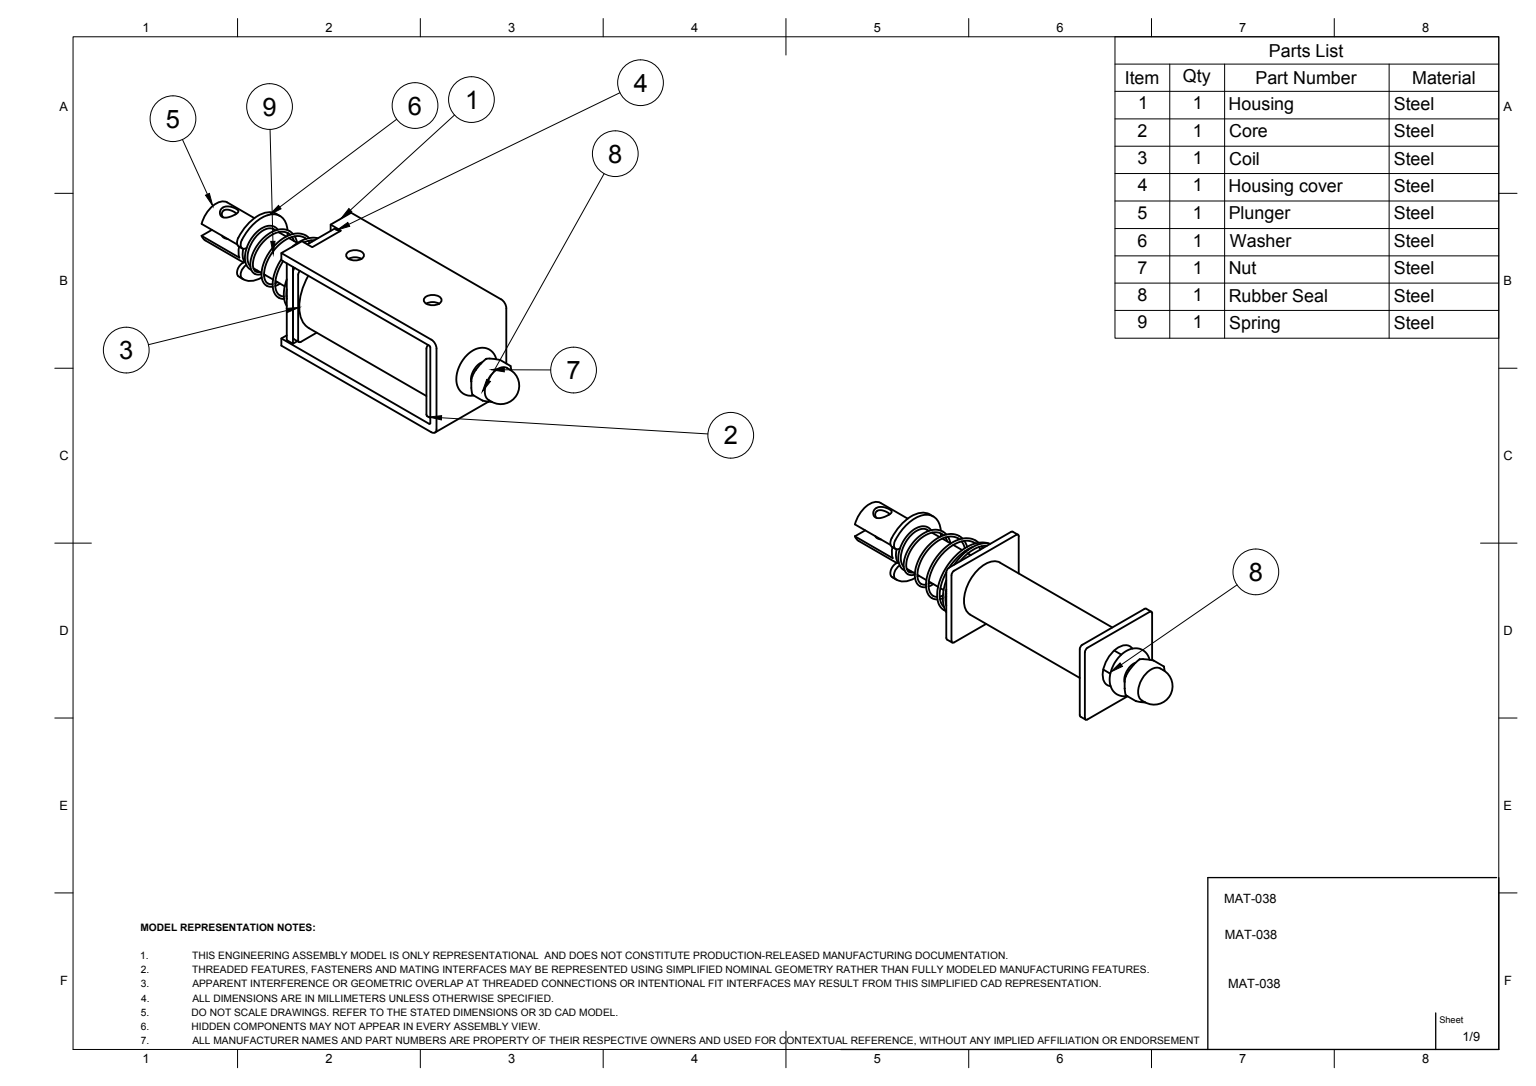
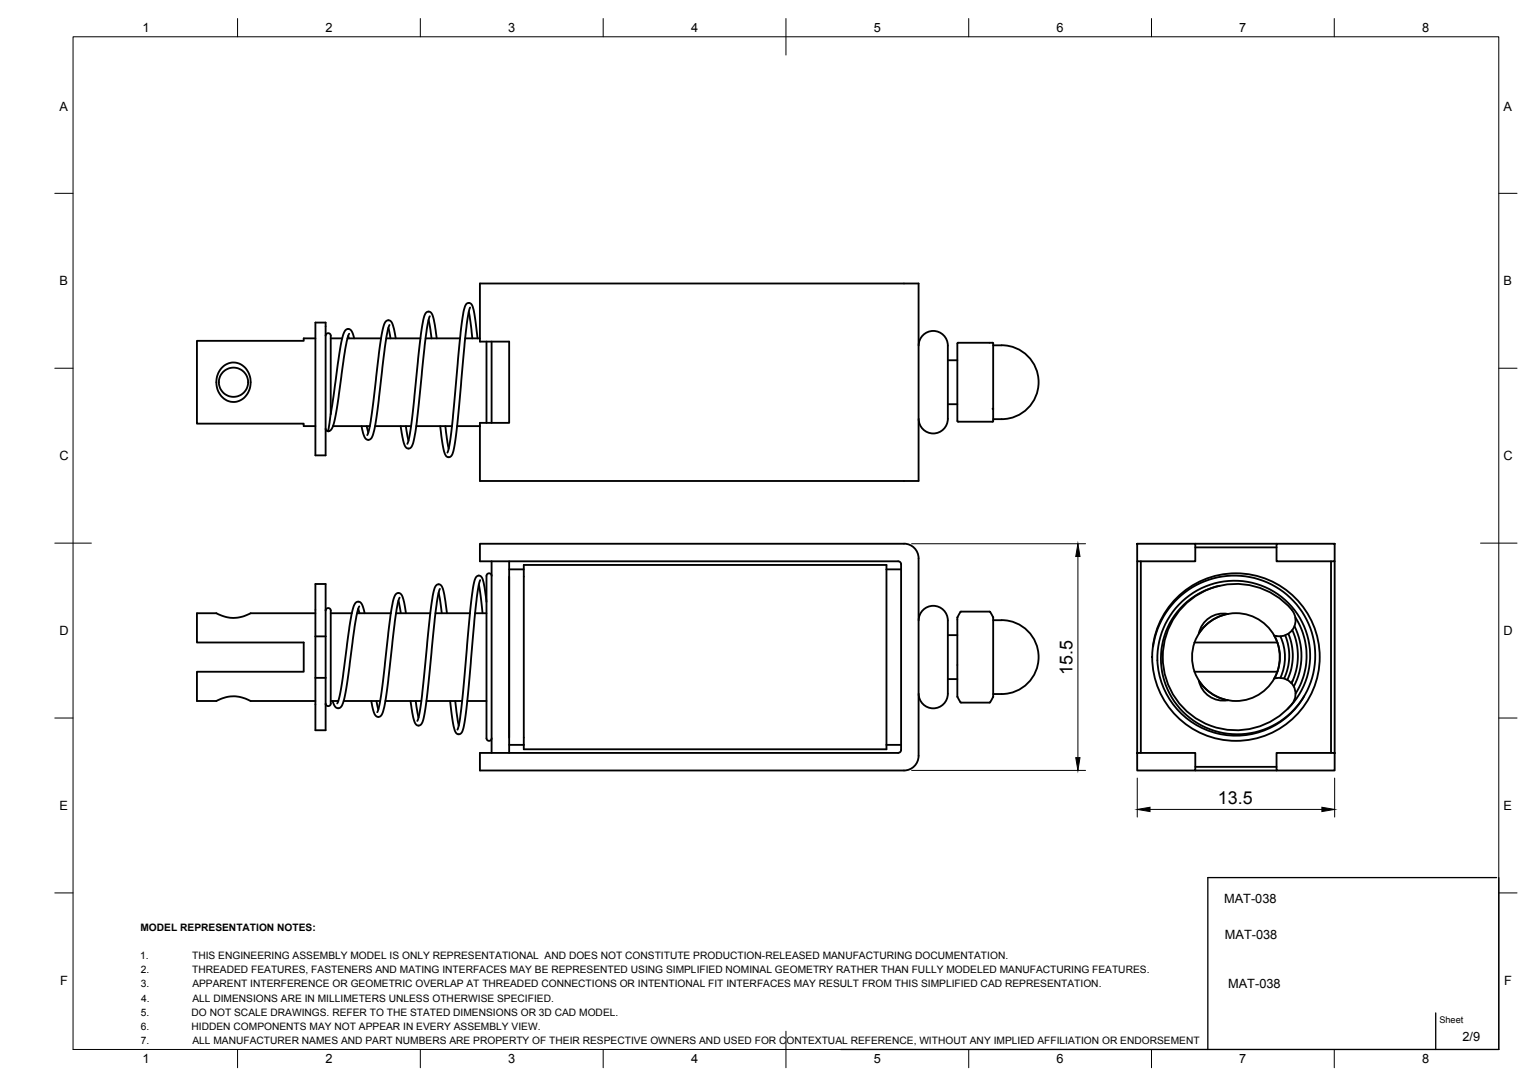
ISO-10303-21;
HEADER;
/* Generated by software containing ST-Developer
 * from STEP Tools, Inc. (www.steptools.com) 
 */

FILE_DESCRIPTION(
/* description */ ('STEP AP214'),
/* implementation_level */ '2;1');

FILE_NAME(
/* name */ 'MAT-038.step',
/* time_stamp */ '2026-11-14T21:32:33-08:00',
/* author */ (''),
/* organization */ (''),
/* preprocessor_version */ 'ST-DEVELOPER v20.2',
/* originating_system */ 'Autodesk Translation Framework v15.17.0.0',
/* authorisation */ '');

FILE_SCHEMA (('AUTOMOTIVE_DESIGN { 1 0 10303 214 3 1 1 }'));
ENDSEC;

DATA;
#10=MECHANICAL_DESIGN_GEOMETRIC_PRESENTATION_REPRESENTATION('',(#177,#178,
#179,#180,#181,#182,#183,#184,#185,#186),#10551);
#11=ITEM_DEFINED_TRANSFORMATION($,$,#3537,#4027);
#12=ITEM_DEFINED_TRANSFORMATION($,$,#3577,#4028);
#13=ITEM_DEFINED_TRANSFORMATION($,$,#3624,#4029);
#14=ITEM_DEFINED_TRANSFORMATION($,$,#3633,#4030);
#15=ITEM_DEFINED_TRANSFORMATION($,$,#3651,#4031);
#16=ITEM_DEFINED_TRANSFORMATION($,$,#3691,#4032);
#17=ITEM_DEFINED_TRANSFORMATION($,$,#3718,#4033);
#18=ITEM_DEFINED_TRANSFORMATION($,$,#4012,#4034);
#19=ITEM_DEFINED_TRANSFORMATION($,$,#4016,#4035);
#20=(
REPRESENTATION_RELATIONSHIP($,$,#10586,#10585)
REPRESENTATION_RELATIONSHIP_WITH_TRANSFORMATION(#11)
SHAPE_REPRESENTATION_RELATIONSHIP()
);
#21=(
REPRESENTATION_RELATIONSHIP($,$,#10587,#10585)
REPRESENTATION_RELATIONSHIP_WITH_TRANSFORMATION(#12)
SHAPE_REPRESENTATION_RELATIONSHIP()
);
#22=(
REPRESENTATION_RELATIONSHIP($,$,#10588,#10585)
REPRESENTATION_RELATIONSHIP_WITH_TRANSFORMATION(#13)
SHAPE_REPRESENTATION_RELATIONSHIP()
);
#23=(
REPRESENTATION_RELATIONSHIP($,$,#10589,#10585)
REPRESENTATION_RELATIONSHIP_WITH_TRANSFORMATION(#14)
SHAPE_REPRESENTATION_RELATIONSHIP()
);
#24=(
REPRESENTATION_RELATIONSHIP($,$,#10590,#10585)
REPRESENTATION_RELATIONSHIP_WITH_TRANSFORMATION(#15)
SHAPE_REPRESENTATION_RELATIONSHIP()
);
#25=(
REPRESENTATION_RELATIONSHIP($,$,#10591,#10585)
REPRESENTATION_RELATIONSHIP_WITH_TRANSFORMATION(#16)
SHAPE_REPRESENTATION_RELATIONSHIP()
);
#26=(
REPRESENTATION_RELATIONSHIP($,$,#10592,#10585)
REPRESENTATION_RELATIONSHIP_WITH_TRANSFORMATION(#17)
SHAPE_REPRESENTATION_RELATIONSHIP()
);
#27=(
REPRESENTATION_RELATIONSHIP($,$,#10593,#10585)
REPRESENTATION_RELATIONSHIP_WITH_TRANSFORMATION(#18)
SHAPE_REPRESENTATION_RELATIONSHIP()
);
#28=(
REPRESENTATION_RELATIONSHIP($,$,#10594,#10585)
REPRESENTATION_RELATIONSHIP_WITH_TRANSFORMATION(#19)
SHAPE_REPRESENTATION_RELATIONSHIP()
);
#29=CONTEXT_DEPENDENT_SHAPE_REPRESENTATION(#20,#10576);
#30=CONTEXT_DEPENDENT_SHAPE_REPRESENTATION(#21,#10577);
#31=CONTEXT_DEPENDENT_SHAPE_REPRESENTATION(#22,#10578);
#32=CONTEXT_DEPENDENT_SHAPE_REPRESENTATION(#23,#10579);
#33=CONTEXT_DEPENDENT_SHAPE_REPRESENTATION(#24,#10580);
#34=CONTEXT_DEPENDENT_SHAPE_REPRESENTATION(#25,#10581);
#35=CONTEXT_DEPENDENT_SHAPE_REPRESENTATION(#26,#10582);
#36=CONTEXT_DEPENDENT_SHAPE_REPRESENTATION(#27,#10583);
#37=CONTEXT_DEPENDENT_SHAPE_REPRESENTATION(#28,#10584);
#38=NEXT_ASSEMBLY_USAGE_OCCURRENCE('Housing:1','Housing:1','Housing:1',
#10596,#10597,'Housing:1');
#39=NEXT_ASSEMBLY_USAGE_OCCURRENCE('Core:1','Core:1','Core:1',#10596,#10598,
'Core:1');
#40=NEXT_ASSEMBLY_USAGE_OCCURRENCE('Coil:1','Coil:1','Coil:1',#10596,#10599,
'Coil:1');
#41=NEXT_ASSEMBLY_USAGE_OCCURRENCE('Housing Cover:1','Housing Cover:1',
'Housing Cover:1',#10596,#10600,'Housing Cover:1');
#42=NEXT_ASSEMBLY_USAGE_OCCURRENCE('Plunger:1','Plunger:1','Plunger:1',
#10596,#10601,'Plunger:1');
#43=NEXT_ASSEMBLY_USAGE_OCCURRENCE('Washer:1','Washer:1','Washer:1',#10596,
#10602,'Washer:1');
#44=NEXT_ASSEMBLY_USAGE_OCCURRENCE('Nut:1','Nut:1','Nut:1',#10596,#10603,
'Nut:1');
#45=NEXT_ASSEMBLY_USAGE_OCCURRENCE('Rubber Seal:1','Rubber Seal:1',
'Rubber Seal:1',#10596,#10604,'Rubber Seal:1');
#46=NEXT_ASSEMBLY_USAGE_OCCURRENCE('Spring:1','Spring:1','Spring:1',#10596,
#10605,'Spring:1');
#47=(
BOUNDED_SURFACE()
B_SPLINE_SURFACE(3,3,((#8436,#8437,#8438,#8439,#8440,#8441,#8442,#8443,
#8444,#8445,#8446,#8447,#8448,#8449,#8450,#8451,#8452,#8453,#8454,#8455,
#8456,#8457,#8458,#8459,#8460,#8461,#8462,#8463,#8464,#8465,#8466,#8467,
#8468,#8469,#8470,#8471,#8472,#8473,#8474,#8475,#8476,#8477,#8478,#8479,
#8480,#8481,#8482,#8483,#8484,#8485,#8486,#8487,#8488,#8489,#8490,#8491,
#8492,#8493,#8494,#8495,#8496,#8497,#8498,#8499,#8500,#8501,#8502,#8503,
#8504,#8505,#8506,#8507,#8508,#8509,#8510,#8511,#8512,#8513,#8514,#8515,
#8516,#8517,#8518,#8519,#8520,#8521,#8522,#8523,#8524,#8525,#8526,#8527,
#8528,#8529,#8530,#8531,#8532,#8533,#8534,#8535,#8536,#8537,#8538,#8539,
#8540,#8541,#8542,#8543,#8544,#8545,#8546,#8547,#8548,#8549,#8550,#8551,
#8552,#8553,#8554,#8555,#8556,#8557,#8558,#8559,#8560,#8561,#8562,#8563,
#8564,#8565),(#8566,#8567,#8568,#8569,#8570,#8571,#8572,#8573,#8574,#8575,
#8576,#8577,#8578,#8579,#8580,#8581,#8582,#8583,#8584,#8585,#8586,#8587,
#8588,#8589,#8590,#8591,#8592,#8593,#8594,#8595,#8596,#8597,#8598,#8599,
#8600,#8601,#8602,#8603,#8604,#8605,#8606,#8607,#8608,#8609,#8610,#8611,
#8612,#8613,#8614,#8615,#8616,#8617,#8618,#8619,#8620,#8621,#8622,#8623,
#8624,#8625,#8626,#8627,#8628,#8629,#8630,#8631,#8632,#8633,#8634,#8635,
#8636,#8637,#8638,#8639,#8640,#8641,#8642,#8643,#8644,#8645,#8646,#8647,
#8648,#8649,#8650,#8651,#8652,#8653,#8654,#8655,#8656,#8657,#8658,#8659,
#8660,#8661,#8662,#8663,#8664,#8665,#8666,#8667,#8668,#8669,#8670,#8671,
#8672,#8673,#8674,#8675,#8676,#8677,#8678,#8679,#8680,#8681,#8682,#8683,
#8684,#8685,#8686,#8687,#8688,#8689,#8690,#8691,#8692,#8693,#8694,#8695),
(#8696,#8697,#8698,#8699,#8700,#8701,#8702,#8703,#8704,#8705,#8706,#8707,
#8708,#8709,#8710,#8711,#8712,#8713,#8714,#8715,#8716,#8717,#8718,#8719,
#8720,#8721,#8722,#8723,#8724,#8725,#8726,#8727,#8728,#8729,#8730,#8731,
#8732,#8733,#8734,#8735,#8736,#8737,#8738,#8739,#8740,#8741,#8742,#8743,
#8744,#8745,#8746,#8747,#8748,#8749,#8750,#8751,#8752,#8753,#8754,#8755,
#8756,#8757,#8758,#8759,#8760,#8761,#8762,#8763,#8764,#8765,#8766,#8767,
#8768,#8769,#8770,#8771,#8772,#8773,#8774,#8775,#8776,#8777,#8778,#8779,
#8780,#8781,#8782,#8783,#8784,#8785,#8786,#8787,#8788,#8789,#8790,#8791,
#8792,#8793,#8794,#8795,#8796,#8797,#8798,#8799,#8800,#8801,#8802,#8803,
#8804,#8805,#8806,#8807,#8808,#8809,#8810,#8811,#8812,#8813,#8814,#8815,
#8816,#8817,#8818,#8819,#8820,#8821,#8822,#8823,#8824,#8825),(#8826,#8827,
#8828,#8829,#8830,#8831,#8832,#8833,#8834,#8835,#8836,#8837,#8838,#8839,
#8840,#8841,#8842,#8843,#8844,#8845,#8846,#8847,#8848,#8849,#8850,#8851,
#8852,#8853,#8854,#8855,#8856,#8857,#8858,#8859,#8860,#8861,#8862,#8863,
#8864,#8865,#8866,#8867,#8868,#8869,#8870,#8871,#8872,#8873,#8874,#8875,
#8876,#8877,#8878,#8879,#8880,#8881,#8882,#8883,#8884,#8885,#8886,#8887,
#8888,#8889,#8890,#8891,#8892,#8893,#8894,#8895,#8896,#8897,#8898,#8899,
#8900,#8901,#8902,#8903,#8904,#8905,#8906,#8907,#8908,#8909,#8910,#8911,
#8912,#8913,#8914,#8915,#8916,#8917,#8918,#8919,#8920,#8921,#8922,#8923,
#8924,#8925,#8926,#8927,#8928,#8929,#8930,#8931,#8932,#8933,#8934,#8935,
#8936,#8937,#8938,#8939,#8940,#8941,#8942,#8943,#8944,#8945,#8946,#8947,
#8948,#8949,#8950,#8951,#8952,#8953,#8954,#8955),(#8956,#8957,#8958,#8959,
#8960,#8961,#8962,#8963,#8964,#8965,#8966,#8967,#8968,#8969,#8970,#8971,
#8972,#8973,#8974,#8975,#8976,#8977,#8978,#8979,#8980,#8981,#8982,#8983,
#8984,#8985,#8986,#8987,#8988,#8989,#8990,#8991,#8992,#8993,#8994,#8995,
#8996,#8997,#8998,#8999,#9000,#9001,#9002,#9003,#9004,#9005,#9006,#9007,
#9008,#9009,#9010,#9011,#9012,#9013,#9014,#9015,#9016,#9017,#9018,#9019,
#9020,#9021,#9022,#9023,#9024,#9025,#9026,#9027,#9028,#9029,#9030,#9031,
#9032,#9033,#9034,#9035,#9036,#9037,#9038,#9039,#9040,#9041,#9042,#9043,
#9044,#9045,#9046,#9047,#9048,#9049,#9050,#9051,#9052,#9053,#9054,#9055,
#9056,#9057,#9058,#9059,#9060,#9061,#9062,#9063,#9064,#9065,#9066,#9067,
#9068,#9069,#9070,#9071,#9072,#9073,#9074,#9075,#9076,#9077,#9078,#9079,
#9080,#9081,#9082,#9083,#9084,#9085),(#9086,#9087,#9088,#9089,#9090,#9091,
#9092,#9093,#9094,#9095,#9096,#9097,#9098,#9099,#9100,#9101,#9102,#9103,
#9104,#9105,#9106,#9107,#9108,#9109,#9110,#9111,#9112,#9113,#9114,#9115,
#9116,#9117,#9118,#9119,#9120,#9121,#9122,#9123,#9124,#9125,#9126,#9127,
#9128,#9129,#9130,#9131,#9132,#9133,#9134,#9135,#9136,#9137,#9138,#9139,
#9140,#9141,#9142,#9143,#9144,#9145,#9146,#9147,#9148,#9149,#9150,#9151,
#9152,#9153,#9154,#9155,#9156,#9157,#9158,#9159,#9160,#9161,#9162,#9163,
#9164,#9165,#9166,#9167,#9168,#9169,#9170,#9171,#9172,#9173,#9174,#9175,
#9176,#9177,#9178,#9179,#9180,#9181,#9182,#9183,#9184,#9185,#9186,#9187,
#9188,#9189,#9190,#9191,#9192,#9193,#9194,#9195,#9196,#9197,#9198,#9199,
#9200,#9201,#9202,#9203,#9204,#9205,#9206,#9207,#9208,#9209,#9210,#9211,
#9212,#9213,#9214,#9215),(#9216,#9217,#9218,#9219,#9220,#9221,#9222,#9223,
#9224,#9225,#9226,#9227,#9228,#9229,#9230,#9231,#9232,#9233,#9234,#9235,
#9236,#9237,#9238,#9239,#9240,#9241,#9242,#9243,#9244,#9245,#9246,#9247,
#9248,#9249,#9250,#9251,#9252,#9253,#9254,#9255,#9256,#9257,#9258,#9259,
#9260,#9261,#9262,#9263,#9264,#9265,#9266,#9267,#9268,#9269,#9270,#9271,
#9272,#9273,#9274,#9275,#9276,#9277,#9278,#9279,#9280,#9281,#9282,#9283,
#9284,#9285,#9286,#9287,#9288,#9289,#9290,#9291,#9292,#9293,#9294,#9295,
#9296,#9297,#9298,#9299,#9300,#9301,#9302,#9303,#9304,#9305,#9306,#9307,
#9308,#9309,#9310,#9311,#9312,#9313,#9314,#9315,#9316,#9317,#9318,#9319,
#9320,#9321,#9322,#9323,#9324,#9325,#9326,#9327,#9328,#9329,#9330,#9331,
#9332,#9333,#9334,#9335,#9336,#9337,#9338,#9339,#9340,#9341,#9342,#9343,
#9344,#9345)),.UNSPECIFIED.,.T.,.F.,.F.)
B_SPLINE_SURFACE_WITH_KNOTS((4,3,4),(4,2,2,2,2,2,2,2,2,2,2,2,2,2,2,2,2,
2,2,2,2,2,2,2,2,2,2,2,2,2,2,2,2,2,2,2,2,2,2,2,2,2,2,2,2,2,2,2,2,2,2,2,2,
2,2,2,2,2,2,2,2,2,2,2,4),(0.,0.5,1.),(-1.6716721247158E-5,0.015625,0.03125,
0.046875,0.0625,0.078125,0.09375,0.109375,0.125,0.140625,0.15625,0.171875,
0.1875,0.203125,0.21875,0.234375,0.25,0.265625,0.28125,0.296875,0.3125,
0.328125,0.34375,0.359375,0.375,0.390625,0.40625,0.421875,0.4375,0.453125,
0.46875,0.484375,0.5,0.515625,0.53125,0.546875,0.5625,0.578125,0.59375,
0.609375,0.625,0.640625,0.65625,0.671875,0.6875,0.703125,0.71875,0.734375,
0.75,0.765625,0.78125,0.796875,0.8125,0.828125,0.84375,0.859375,0.875,0.890625,
0.90625,0.921875,0.9375,0.953125,0.96875,0.984375,1.),.UNSPECIFIED.)
GEOMETRIC_REPRESENTATION_ITEM()
RATIONAL_B_SPLINE_SURFACE(((1.,1.,1.,1.,1.,1.,1.,1.,1.,1.,1.,1.,1.,1.,1.,
1.,1.,1.,1.,1.,1.,1.,1.,1.,1.,1.,1.,1.,1.,1.,1.,1.,1.,1.,1.,1.,1.,1.,1.,
1.,1.,1.,1.,1.,1.,1.,1.,1.,1.,1.,1.,1.,1.,1.,1.,1.,1.,1.,1.,1.,1.,1.,1.,
1.,1.,1.,1.,1.,1.,1.,1.,1.,1.,1.,1.,1.,1.,1.,1.,1.,1.,1.,1.,1.,1.,1.,1.,
1.,1.,1.,1.,1.,1.,1.,1.,1.,1.,1.,1.,1.,1.,1.,1.,1.,1.,1.,1.,1.,1.,1.,1.,
1.,1.,1.,1.,1.,1.,1.,1.,1.,1.,1.,1.,1.,1.,1.,1.,1.,1.,1.),(0.333333333333334,
0.333333333333333,0.333333333333333,0.333333333333333,0.333333333333333,
0.333333333333333,0.333333333333333,0.333333333333333,0.333333333333333,
0.333333333333333,0.333333333333333,0.333333333333333,0.333333333333333,
0.333333333333333,0.333333333333333,0.333333333333333,0.333333333333333,
0.333333333333333,0.333333333333333,0.333333333333333,0.333333333333333,
0.333333333333333,0.333333333333333,0.333333333333333,0.333333333333333,
0.333333333333333,0.333333333333333,0.333333333333333,0.333333333333333,
0.333333333333333,0.333333333333333,0.333333333333333,0.333333333333333,
0.333333333333333,0.333333333333333,0.333333333333333,0.333333333333333,
0.333333333333333,0.333333333333333,0.333333333333333,0.333333333333333,
0.333333333333333,0.333333333333333,0.333333333333333,0.333333333333333,
0.333333333333333,0.333333333333333,0.333333333333333,0.333333333333333,
0.333333333333333,0.333333333333333,0.333333333333333,0.333333333333333,
0.333333333333333,0.333333333333333,0.333333333333333,0.333333333333333,
0.333333333333333,0.333333333333333,0.333333333333333,0.333333333333333,
0.333333333333333,0.333333333333333,0.333333333333333,0.333333333333333,
0.333333333333333,0.333333333333333,0.333333333333333,0.333333333333333,
0.333333333333333,0.333333333333333,0.333333333333333,0.333333333333333,
0.333333333333333,0.333333333333333,0.333333333333333,0.333333333333333,
0.333333333333333,0.333333333333333,0.333333333333333,0.333333333333333,
0.333333333333333,0.333333333333333,0.333333333333333,0.333333333333333,
0.333333333333333,0.333333333333333,0.333333333333333,0.333333333333333,
0.333333333333333,0.333333333333333,0.333333333333333,0.333333333333333,
0.333333333333333,0.333333333333333,0.333333333333333,0.333333333333333,
0.333333333333333,0.333333333333333,0.333333333333333,0.333333333333333,
0.333333333333333,0.333333333333333,0.333333333333333,0.333333333333333,
0.333333333333333,0.333333333333333,0.333333333333333,0.333333333333333,
0.333333333333333,0.333333333333333,0.333333333333333,0.333333333333333,
0.333333333333333,0.333333333333333,0.333333333333333,0.333333333333333,
0.333333333333333,0.333333333333333,0.333333333333333,0.333333333333333,
0.333333333333333,0.333333333333333,0.333333333333333,0.333333333333333,
0.333333333333333,0.333333333333333,0.333333333333333,0.333333333333333,
0.333333333333333),(0.333333333333334,0.333333333333333,0.333333333333333,
0.333333333333333,0.333333333333333,0.333333333333333,0.333333333333333,
0.333333333333333,0.333333333333333,0.333333333333333,0.333333333333333,
0.333333333333333,0.333333333333333,0.333333333333333,0.333333333333333,
0.333333333333333,0.333333333333333,0.333333333333333,0.333333333333333,
0.333333333333333,0.333333333333333,0.333333333333333,0.333333333333333,
0.333333333333333,0.333333333333333,0.333333333333333,0.333333333333333,
0.333333333333333,0.333333333333333,0.333333333333333,0.333333333333333,
0.333333333333333,0.333333333333333,0.333333333333333,0.333333333333333,
0.333333333333333,0.333333333333333,0.333333333333333,0.333333333333333,
0.333333333333333,0.333333333333333,0.333333333333333,0.333333333333333,
0.333333333333333,0.333333333333333,0.333333333333333,0.333333333333333,
0.333333333333333,0.333333333333333,0.333333333333333,0.333333333333333,
0.333333333333333,0.333333333333333,0.333333333333333,0.333333333333333,
0.333333333333333,0.333333333333333,0.333333333333333,0.333333333333333,
0.333333333333333,0.333333333333333,0.333333333333333,0.333333333333333,
0.333333333333333,0.333333333333333,0.333333333333333,0.333333333333333,
0.333333333333333,0.333333333333333,0.333333333333333,0.333333333333333,
0.333333333333333,0.333333333333333,0.333333333333333,0.333333333333333,
0.333333333333333,0.333333333333333,0.333333333333333,0.333333333333333,
0.333333333333333,0.333333333333333,0.333333333333333,0.333333333333333,
0.333333333333333,0.333333333333333,0.333333333333333,0.333333333333333,
0.333333333333333,0.333333333333333,0.333333333333333,0.333333333333333,
0.333333333333333,0.333333333333333,0.333333333333333,0.333333333333333,
0.333333333333333,0.333333333333333,0.333333333333333,0.333333333333333,
0.333333333333333,0.333333333333333,0.333333333333333,0.333333333333333,
0.333333333333333,0.333333333333333,0.333333333333333,0.333333333333333,
0.333333333333333,0.333333333333333,0.333333333333333,0.333333333333333,
0.333333333333333,0.333333333333333,0.333333333333333,0.333333333333333,
0.333333333333333,0.333333333333333,0.333333333333333,0.333333333333333,
0.333333333333333,0.333333333333333,0.333333333333333,0.333333333333333,
0.333333333333333,0.333333333333333,0.333333333333333,0.333333333333333,
0.333333333333333,0.333333333333333,0.333333333333333),(1.,1.,1.,1.,1.,
1.,1.,1.,1.,1.,1.,1.,1.,1.,1.,1.,1.,1.,1.,1.,1.,1.,1.,1.,1.,1.,1.,1.,1.,
1.,1.,1.,1.,1.,1.,1.,1.,1.,1.,1.,1.,1.,1.,1.,1.,1.,1.,1.,1.,1.,1.,1.,1.,
1.,1.,1.,1.,1.,1.,1.,1.,1.,1.,1.,1.,1.,1.,1.,1.,1.,1.,1.,1.,1.,1.,1.,1.,
1.,1.,1.,1.,1.,1.,1.,1.,1.,1.,1.,1.,1.,1.,1.,1.,1.,1.,1.,1.,1.,1.,1.,1.,
1.,1.,1.,1.,1.,1.,1.,1.,1.,1.,1.,1.,1.,1.,1.,1.,1.,1.,1.,1.,1.,1.,1.,1.,
1.,1.,1.,1.,1.),(0.333333333333334,0.333333333333333,0.333333333333333,
0.333333333333333,0.333333333333333,0.333333333333333,0.333333333333333,
0.333333333333333,0.333333333333333,0.333333333333333,0.333333333333333,
0.333333333333333,0.333333333333333,0.333333333333333,0.333333333333333,
0.333333333333333,0.333333333333333,0.333333333333333,0.333333333333333,
0.333333333333333,0.333333333333333,0.333333333333333,0.333333333333333,
0.333333333333333,0.333333333333333,0.333333333333333,0.333333333333333,
0.333333333333333,0.333333333333333,0.333333333333333,0.333333333333333,
0.333333333333333,0.333333333333333,0.333333333333333,0.333333333333333,
0.333333333333333,0.333333333333333,0.333333333333333,0.333333333333333,
0.333333333333333,0.333333333333333,0.333333333333333,0.333333333333333,
0.333333333333333,0.333333333333333,0.333333333333333,0.333333333333333,
0.333333333333333,0.333333333333333,0.333333333333333,0.333333333333333,
0.333333333333333,0.333333333333333,0.333333333333333,0.333333333333333,
0.333333333333333,0.333333333333333,0.333333333333333,0.333333333333333,
0.333333333333333,0.333333333333333,0.333333333333333,0.333333333333333,
0.333333333333333,0.333333333333333,0.333333333333333,0.333333333333333,
0.333333333333333,0.333333333333333,0.333333333333333,0.333333333333333,
0.333333333333333,0.333333333333333,0.333333333333333,0.333333333333333,
0.333333333333333,0.333333333333333,0.333333333333333,0.333333333333333,
0.333333333333333,0.333333333333333,0.333333333333333,0.333333333333333,
0.333333333333333,0.333333333333333,0.333333333333333,0.333333333333333,
0.333333333333333,0.333333333333333,0.333333333333333,0.333333333333333,
0.333333333333333,0.333333333333333,0.333333333333333,0.333333333333333,
0.333333333333333,0.333333333333333,0.333333333333333,0.333333333333333,
0.333333333333333,0.333333333333333,0.333333333333333,0.333333333333333,
0.333333333333333,0.333333333333333,0.333333333333333,0.333333333333333,
0.333333333333333,0.333333333333333,0.333333333333333,0.333333333333333,
0.333333333333333,0.333333333333333,0.333333333333333,0.333333333333333,
0.333333333333333,0.333333333333333,0.333333333333333,0.333333333333333,
0.333333333333333,0.333333333333333,0.333333333333333,0.333333333333333,
0.333333333333333,0.333333333333333,0.333333333333333,0.333333333333333,
0.333333333333333,0.333333333333333,0.333333333333333),(0.333333333333334,
0.333333333333333,0.333333333333333,0.333333333333333,0.333333333333333,
0.333333333333333,0.333333333333333,0.333333333333333,0.333333333333333,
0.333333333333333,0.333333333333333,0.333333333333333,0.333333333333333,
0.333333333333333,0.333333333333333,0.333333333333333,0.333333333333333,
0.333333333333333,0.333333333333333,0.333333333333333,0.333333333333333,
0.333333333333333,0.333333333333333,0.333333333333333,0.333333333333333,
0.333333333333333,0.333333333333333,0.333333333333333,0.333333333333333,
0.333333333333333,0.333333333333333,0.333333333333333,0.333333333333333,
0.333333333333333,0.333333333333333,0.333333333333333,0.333333333333333,
0.333333333333333,0.333333333333333,0.333333333333333,0.333333333333333,
0.333333333333333,0.333333333333333,0.333333333333333,0.333333333333333,
0.333333333333333,0.333333333333333,0.333333333333333,0.333333333333333,
0.333333333333333,0.333333333333333,0.333333333333333,0.333333333333333,
0.333333333333333,0.333333333333333,0.333333333333333,0.333333333333333,
0.333333333333333,0.333333333333333,0.333333333333333,0.333333333333333,
0.333333333333333,0.333333333333333,0.333333333333333,0.333333333333333,
0.333333333333333,0.333333333333333,0.333333333333333,0.333333333333333,
0.333333333333333,0.333333333333333,0.333333333333333,0.333333333333333,
0.333333333333333,0.333333333333333,0.333333333333333,0.333333333333333,
0.333333333333333,0.333333333333333,0.333333333333333,0.333333333333333,
0.333333333333333,0.333333333333333,0.333333333333333,0.333333333333333,
0.333333333333333,0.333333333333333,0.333333333333333,0.333333333333333,
0.333333333333333,0.333333333333333,0.333333333333333,0.333333333333333,
0.333333333333333,0.333333333333333,0.333333333333333,0.333333333333333,
0.333333333333333,0.333333333333333,0.333333333333333,0.333333333333333,
0.333333333333333,0.333333333333333,0.333333333333333,0.333333333333333,
0.333333333333333,0.333333333333333,0.333333333333333,0.333333333333333,
0.333333333333333,0.333333333333333,0.333333333333333,0.333333333333333,
0.333333333333333,0.333333333333333,0.333333333333333,0.333333333333333,
0.333333333333333,0.333333333333333,0.333333333333333,0.333333333333333,
0.333333333333333,0.333333333333333,0.333333333333333,0.333333333333333,
0.333333333333333,0.333333333333333,0.333333333333333,0.333333333333333,
0.333333333333333),(1.,1.,1.,1.,1.,1.,1.,1.,1.,1.,1.,1.,1.,1.,1.,1.,1.,
1.,1.,1.,1.,1.,1.,1.,1.,1.,1.,1.,1.,1.,1.,1.,1.,1.,1.,1.,1.,1.,1.,1.,1.,
1.,1.,1.,1.,1.,1.,1.,1.,1.,1.,1.,1.,1.,1.,1.,1.,1.,1.,1.,1.,1.,1.,1.,1.,
1.,1.,1.,1.,1.,1.,1.,1.,1.,1.,1.,1.,1.,1.,1.,1.,1.,1.,1.,1.,1.,1.,1.,1.,
1.,1.,1.,1.,1.,1.,1.,1.,1.,1.,1.,1.,1.,1.,1.,1.,1.,1.,1.,1.,1.,1.,1.,1.,
1.,1.,1.,1.,1.,1.,1.,1.,1.,1.,1.,1.,1.,1.,1.,1.,1.)))
REPRESENTATION_ITEM('')
SURFACE()
);
#48=(
BOUNDED_SURFACE()
B_SPLINE_SURFACE(3,3,((#9609,#9610,#9611,#9612,#9613,#9614,#9615,#9616,
#9617,#9618,#9619,#9620,#9621,#9622,#9623,#9624,#9625,#9626,#9627,#9628,
#9629,#9630,#9631,#9632,#9633,#9634,#9635,#9636,#9637,#9638,#9639,#9640,
#9641,#9642,#9643,#9644,#9645,#9646,#9647,#9648,#9649,#9650,#9651,#9652,
#9653,#9654,#9655,#9656,#9657,#9658,#9659,#9660,#9661,#9662,#9663,#9664,
#9665,#9666,#9667,#9668,#9669,#9670,#9671,#9672,#9673,#9674,#9675,#9676,
#9677,#9678,#9679,#9680,#9681,#9682,#9683,#9684,#9685,#9686,#9687,#9688,
#9689,#9690,#9691,#9692,#9693,#9694,#9695,#9696,#9697,#9698,#9699,#9700,
#9701,#9702,#9703,#9704,#9705,#9706,#9707,#9708,#9709,#9710,#9711,#9712,
#9713,#9714,#9715,#9716,#9717,#9718,#9719,#9720,#9721,#9722,#9723,#9724,
#9725,#9726,#9727,#9728,#9729,#9730,#9731,#9732,#9733,#9734,#9735,#9736,
#9737,#9738),(#9739,#9740,#9741,#9742,#9743,#9744,#9745,#9746,#9747,#9748,
#9749,#9750,#9751,#9752,#9753,#9754,#9755,#9756,#9757,#9758,#9759,#9760,
#9761,#9762,#9763,#9764,#9765,#9766,#9767,#9768,#9769,#9770,#9771,#9772,
#9773,#9774,#9775,#9776,#9777,#9778,#9779,#9780,#9781,#9782,#9783,#9784,
#9785,#9786,#9787,#9788,#9789,#9790,#9791,#9792,#9793,#9794,#9795,#9796,
#9797,#9798,#9799,#9800,#9801,#9802,#9803,#9804,#9805,#9806,#9807,#9808,
#9809,#9810,#9811,#9812,#9813,#9814,#9815,#9816,#9817,#9818,#9819,#9820,
#9821,#9822,#9823,#9824,#9825,#9826,#9827,#9828,#9829,#9830,#9831,#9832,
#9833,#9834,#9835,#9836,#9837,#9838,#9839,#9840,#9841,#9842,#9843,#9844,
#9845,#9846,#9847,#9848,#9849,#9850,#9851,#9852,#9853,#9854,#9855,#9856,
#9857,#9858,#9859,#9860,#9861,#9862,#9863,#9864,#9865,#9866,#9867,#9868),
(#9869,#9870,#9871,#9872,#9873,#9874,#9875,#9876,#9877,#9878,#9879,#9880,
#9881,#9882,#9883,#9884,#9885,#9886,#9887,#9888,#9889,#9890,#9891,#9892,
#9893,#9894,#9895,#9896,#9897,#9898,#9899,#9900,#9901,#9902,#9903,#9904,
#9905,#9906,#9907,#9908,#9909,#9910,#9911,#9912,#9913,#9914,#9915,#9916,
#9917,#9918,#9919,#9920,#9921,#9922,#9923,#9924,#9925,#9926,#9927,#9928,
#9929,#9930,#9931,#9932,#9933,#9934,#9935,#9936,#9937,#9938,#9939,#9940,
#9941,#9942,#9943,#9944,#9945,#9946,#9947,#9948,#9949,#9950,#9951,#9952,
#9953,#9954,#9955,#9956,#9957,#9958,#9959,#9960,#9961,#9962,#9963,#9964,
#9965,#9966,#9967,#9968,#9969,#9970,#9971,#9972,#9973,#9974,#9975,#9976,
#9977,#9978,#9979,#9980,#9981,#9982,#9983,#9984,#9985,#9986,#9987,#9988,
#9989,#9990,#9991,#9992,#9993,#9994,#9995,#9996,#9997,#9998),(#9999,#10000,
#10001,#10002,#10003,#10004,#10005,#10006,#10007,#10008,#10009,#10010,#10011,
#10012,#10013,#10014,#10015,#10016,#10017,#10018,#10019,#10020,#10021,#10022,
#10023,#10024,#10025,#10026,#10027,#10028,#10029,#10030,#10031,#10032,#10033,
#10034,#10035,#10036,#10037,#10038,#10039,#10040,#10041,#10042,#10043,#10044,
#10045,#10046,#10047,#10048,#10049,#10050,#10051,#10052,#10053,#10054,#10055,
#10056,#10057,#10058,#10059,#10060,#10061,#10062,#10063,#10064,#10065,#10066,
#10067,#10068,#10069,#10070,#10071,#10072,#10073,#10074,#10075,#10076,#10077,
#10078,#10079,#10080,#10081,#10082,#10083,#10084,#10085,#10086,#10087,#10088,
#10089,#10090,#10091,#10092,#10093,#10094,#10095,#10096,#10097,#10098,#10099,
#10100,#10101,#10102,#10103,#10104,#10105,#10106,#10107,#10108,#10109,#10110,
#10111,#10112,#10113,#10114,#10115,#10116,#10117,#10118,#10119,#10120,#10121,
#10122,#10123,#10124,#10125,#10126,#10127,#10128),(#10129,#10130,#10131,
#10132,#10133,#10134,#10135,#10136,#10137,#10138,#10139,#10140,#10141,#10142,
#10143,#10144,#10145,#10146,#10147,#10148,#10149,#10150,#10151,#10152,#10153,
#10154,#10155,#10156,#10157,#10158,#10159,#10160,#10161,#10162,#10163,#10164,
#10165,#10166,#10167,#10168,#10169,#10170,#10171,#10172,#10173,#10174,#10175,
#10176,#10177,#10178,#10179,#10180,#10181,#10182,#10183,#10184,#10185,#10186,
#10187,#10188,#10189,#10190,#10191,#10192,#10193,#10194,#10195,#10196,#10197,
#10198,#10199,#10200,#10201,#10202,#10203,#10204,#10205,#10206,#10207,#10208,
#10209,#10210,#10211,#10212,#10213,#10214,#10215,#10216,#10217,#10218,#10219,
#10220,#10221,#10222,#10223,#10224,#10225,#10226,#10227,#10228,#10229,#10230,
#10231,#10232,#10233,#10234,#10235,#10236,#10237,#10238,#10239,#10240,#10241,
#10242,#10243,#10244,#10245,#10246,#10247,#10248,#10249,#10250,#10251,#10252,
#10253,#10254,#10255,#10256,#10257,#10258),(#10259,#10260,#10261,#10262,
#10263,#10264,#10265,#10266,#10267,#10268,#10269,#10270,#10271,#10272,#10273,
#10274,#10275,#10276,#10277,#10278,#10279,#10280,#10281,#10282,#10283,#10284,
#10285,#10286,#10287,#10288,#10289,#10290,#10291,#10292,#10293,#10294,#10295,
#10296,#10297,#10298,#10299,#10300,#10301,#10302,#10303,#10304,#10305,#10306,
#10307,#10308,#10309,#10310,#10311,#10312,#10313,#10314,#10315,#10316,#10317,
#10318,#10319,#10320,#10321,#10322,#10323,#10324,#10325,#10326,#10327,#10328,
#10329,#10330,#10331,#10332,#10333,#10334,#10335,#10336,#10337,#10338,#10339,
#10340,#10341,#10342,#10343,#10344,#10345,#10346,#10347,#10348,#10349,#10350,
#10351,#10352,#10353,#10354,#10355,#10356,#10357,#10358,#10359,#10360,#10361,
#10362,#10363,#10364,#10365,#10366,#10367,#10368,#10369,#10370,#10371,#10372,
#10373,#10374,#10375,#10376,#10377,#10378,#10379,#10380,#10381,#10382,#10383,
#10384,#10385,#10386,#10387,#10388),(#10389,#10390,#10391,#10392,#10393,
#10394,#10395,#10396,#10397,#10398,#10399,#10400,#10401,#10402,#10403,#10404,
#10405,#10406,#10407,#10408,#10409,#10410,#10411,#10412,#10413,#10414,#10415,
#10416,#10417,#10418,#10419,#10420,#10421,#10422,#10423,#10424,#10425,#10426,
#10427,#10428,#10429,#10430,#10431,#10432,#10433,#10434,#10435,#10436,#10437,
#10438,#10439,#10440,#10441,#10442,#10443,#10444,#10445,#10446,#10447,#10448,
#10449,#10450,#10451,#10452,#10453,#10454,#10455,#10456,#10457,#10458,#10459,
#10460,#10461,#10462,#10463,#10464,#10465,#10466,#10467,#10468,#10469,#10470,
#10471,#10472,#10473,#10474,#10475,#10476,#10477,#10478,#10479,#10480,#10481,
#10482,#10483,#10484,#10485,#10486,#10487,#10488,#10489,#10490,#10491,#10492,
#10493,#10494,#10495,#10496,#10497,#10498,#10499,#10500,#10501,#10502,#10503,
#10504,#10505,#10506,#10507,#10508,#10509,#10510,#10511,#10512,#10513,#10514,
#10515,#10516,#10517,#10518)),.UNSPECIFIED.,.T.,.F.,.F.)
B_SPLINE_SURFACE_WITH_KNOTS((4,3,4),(4,2,2,2,2,2,2,2,2,2,2,2,2,2,2,2,2,
2,2,2,2,2,2,2,2,2,2,2,2,2,2,2,2,2,2,2,2,2,2,2,2,2,2,2,2,2,2,2,2,2,2,2,2,
2,2,2,2,2,2,2,2,2,2,2,4),(0.,0.5,1.),(0.,0.015625,0.03125,0.046875,0.0625,
0.078125,0.09375,0.109375,0.125,0.140625,0.15625,0.171875,0.1875,0.203125,
0.21875,0.234375,0.25,0.265625,0.28125,0.296875,0.3125,0.328125,0.34375,
0.359375,0.375,0.390625,0.40625,0.421875,0.4375,0.453125,0.46875,0.484375,
0.5,0.515625,0.53125,0.546875,0.5625,0.578125,0.59375,0.609375,0.625,0.640625,
0.65625,0.671875,0.6875,0.703125,0.71875,0.734375,0.75,0.765625,0.78125,
0.796875,0.8125,0.828125,0.84375,0.859375,0.875,0.890625,0.90625,0.921875,
0.9375,0.953125,0.96875,0.984375,1.),.UNSPECIFIED.)
GEOMETRIC_REPRESENTATION_ITEM()
RATIONAL_B_SPLINE_SURFACE(((1.,1.,1.,1.,1.,1.,1.,1.,1.,1.,1.,1.,1.,1.,1.,
1.,1.,1.,1.,1.,1.,1.,1.,1.,1.,1.,1.,1.,1.,1.,1.,1.,1.,1.,1.,1.,1.,1.,1.,
1.,1.,1.,1.,1.,1.,1.,1.,1.,1.,1.,1.,1.,1.,1.,1.,1.,1.,1.,1.,1.,1.,1.,1.,
1.,1.,1.,1.,1.,1.,1.,1.,1.,1.,1.,1.,1.,1.,1.,1.,1.,1.,1.,1.,1.,1.,1.,1.,
1.,1.,1.,1.,1.,1.,1.,1.,1.,1.,1.,1.,1.,1.,1.,1.,1.,1.,1.,1.,1.,1.,1.,1.,
1.,1.,1.,1.,1.,1.,1.,1.,1.,1.,1.,1.,1.,1.,1.,1.,1.,1.,1.),(0.333333333333333,
0.333333333333333,0.333333333333333,0.333333333333333,0.333333333333333,
0.333333333333333,0.333333333333333,0.333333333333333,0.333333333333333,
0.333333333333333,0.333333333333333,0.333333333333333,0.333333333333333,
0.333333333333333,0.333333333333333,0.333333333333333,0.333333333333333,
0.333333333333333,0.333333333333333,0.333333333333333,0.333333333333333,
0.333333333333333,0.333333333333333,0.333333333333333,0.333333333333333,
0.333333333333333,0.333333333333333,0.333333333333333,0.333333333333333,
0.333333333333333,0.333333333333333,0.333333333333333,0.333333333333333,
0.333333333333333,0.333333333333333,0.333333333333333,0.333333333333333,
0.333333333333333,0.333333333333333,0.333333333333333,0.333333333333333,
0.333333333333333,0.333333333333333,0.333333333333333,0.333333333333333,
0.333333333333333,0.333333333333333,0.333333333333333,0.333333333333333,
0.333333333333333,0.333333333333333,0.333333333333333,0.333333333333333,
0.333333333333333,0.333333333333333,0.333333333333333,0.333333333333333,
0.333333333333333,0.333333333333333,0.333333333333333,0.333333333333333,
0.333333333333333,0.333333333333333,0.333333333333333,0.333333333333333,
0.333333333333333,0.333333333333333,0.333333333333333,0.333333333333333,
0.333333333333333,0.333333333333333,0.333333333333333,0.333333333333333,
0.333333333333333,0.333333333333333,0.333333333333333,0.333333333333333,
0.333333333333333,0.333333333333333,0.333333333333333,0.333333333333333,
0.333333333333333,0.333333333333333,0.333333333333333,0.333333333333333,
0.333333333333333,0.333333333333333,0.333333333333333,0.333333333333333,
0.333333333333333,0.333333333333333,0.333333333333333,0.333333333333333,
0.333333333333333,0.333333333333333,0.333333333333333,0.333333333333333,
0.333333333333333,0.333333333333333,0.333333333333333,0.333333333333333,
0.333333333333333,0.333333333333333,0.333333333333333,0.333333333333333,
0.333333333333333,0.333333333333333,0.333333333333333,0.333333333333333,
0.333333333333333,0.333333333333333,0.333333333333333,0.333333333333333,
0.333333333333333,0.333333333333333,0.333333333333333,0.333333333333333,
0.333333333333333,0.333333333333333,0.333333333333333,0.333333333333333,
0.333333333333333,0.333333333333333,0.333333333333333,0.333333333333333,
0.333333333333333,0.333333333333333,0.333333333333333,0.333333333333333,
0.333333333333333),(0.333333333333333,0.333333333333333,0.333333333333333,
0.333333333333333,0.333333333333333,0.333333333333333,0.333333333333333,
0.333333333333333,0.333333333333333,0.333333333333333,0.333333333333333,
0.333333333333333,0.333333333333333,0.333333333333333,0.333333333333333,
0.333333333333333,0.333333333333333,0.333333333333333,0.333333333333333,
0.333333333333333,0.333333333333333,0.333333333333333,0.333333333333333,
0.333333333333333,0.333333333333333,0.333333333333333,0.333333333333333,
0.333333333333333,0.333333333333333,0.333333333333333,0.333333333333333,
0.333333333333333,0.333333333333333,0.333333333333333,0.333333333333333,
0.333333333333333,0.333333333333333,0.333333333333333,0.333333333333333,
0.333333333333333,0.333333333333333,0.333333333333333,0.333333333333333,
0.333333333333333,0.333333333333333,0.333333333333333,0.333333333333333,
0.333333333333333,0.333333333333333,0.333333333333333,0.333333333333333,
0.333333333333333,0.333333333333333,0.333333333333333,0.333333333333333,
0.333333333333333,0.333333333333333,0.333333333333333,0.333333333333333,
0.333333333333333,0.333333333333333,0.333333333333333,0.333333333333333,
0.333333333333333,0.333333333333333,0.333333333333333,0.333333333333333,
0.333333333333333,0.333333333333333,0.333333333333333,0.333333333333333,
0.333333333333333,0.333333333333333,0.333333333333333,0.333333333333333,
0.333333333333333,0.333333333333333,0.333333333333333,0.333333333333333,
0.333333333333333,0.333333333333333,0.333333333333333,0.333333333333333,
0.333333333333333,0.333333333333333,0.333333333333333,0.333333333333333,
0.333333333333333,0.333333333333333,0.333333333333333,0.333333333333333,
0.333333333333333,0.333333333333333,0.333333333333333,0.333333333333333,
0.333333333333333,0.333333333333333,0.333333333333333,0.333333333333333,
0.333333333333333,0.333333333333333,0.333333333333333,0.333333333333333,
0.333333333333333,0.333333333333333,0.333333333333333,0.333333333333333,
0.333333333333333,0.333333333333333,0.333333333333333,0.333333333333333,
0.333333333333333,0.333333333333333,0.333333333333333,0.333333333333333,
0.333333333333333,0.333333333333333,0.333333333333333,0.333333333333333,
0.333333333333333,0.333333333333333,0.333333333333333,0.333333333333333,
0.333333333333333,0.333333333333333,0.333333333333333,0.333333333333333,
0.333333333333333,0.333333333333333,0.333333333333333),(1.,1.,1.,1.,1.,
1.,1.,1.,1.,1.,1.,1.,1.,1.,1.,1.,1.,1.,1.,1.,1.,1.,1.,1.,1.,1.,1.,1.,1.,
1.,1.,1.,1.,1.,1.,1.,1.,1.,1.,1.,1.,1.,1.,1.,1.,1.,1.,1.,1.,1.,1.,1.,1.,
1.,1.,1.,1.,1.,1.,1.,1.,1.,1.,1.,1.,1.,1.,1.,1.,1.,1.,1.,1.,1.,1.,1.,1.,
1.,1.,1.,1.,1.,1.,1.,1.,1.,1.,1.,1.,1.,1.,1.,1.,1.,1.,1.,1.,1.,1.,1.,1.,
1.,1.,1.,1.,1.,1.,1.,1.,1.,1.,1.,1.,1.,1.,1.,1.,1.,1.,1.,1.,1.,1.,1.,1.,
1.,1.,1.,1.,1.),(0.333333333333333,0.333333333333333,0.333333333333333,
0.333333333333333,0.333333333333333,0.333333333333333,0.333333333333333,
0.333333333333333,0.333333333333333,0.333333333333333,0.333333333333333,
0.333333333333333,0.333333333333333,0.333333333333333,0.333333333333333,
0.333333333333333,0.333333333333333,0.333333333333333,0.333333333333333,
0.333333333333333,0.333333333333333,0.333333333333333,0.333333333333333,
0.333333333333333,0.333333333333333,0.333333333333333,0.333333333333333,
0.333333333333333,0.333333333333333,0.333333333333333,0.333333333333333,
0.333333333333333,0.333333333333333,0.333333333333333,0.333333333333333,
0.333333333333333,0.333333333333333,0.333333333333333,0.333333333333333,
0.333333333333333,0.333333333333333,0.333333333333333,0.333333333333333,
0.333333333333333,0.333333333333333,0.333333333333333,0.333333333333333,
0.333333333333333,0.333333333333333,0.333333333333333,0.333333333333333,
0.333333333333333,0.333333333333333,0.333333333333333,0.333333333333333,
0.333333333333333,0.333333333333333,0.333333333333333,0.333333333333333,
0.333333333333333,0.333333333333333,0.333333333333333,0.333333333333333,
0.333333333333333,0.333333333333333,0.333333333333333,0.333333333333333,
0.333333333333333,0.333333333333333,0.333333333333333,0.333333333333333,
0.333333333333333,0.333333333333333,0.333333333333333,0.333333333333333,
0.333333333333333,0.333333333333333,0.333333333333333,0.333333333333333,
0.333333333333333,0.333333333333333,0.333333333333333,0.333333333333333,
0.333333333333333,0.333333333333333,0.333333333333333,0.333333333333333,
0.333333333333333,0.333333333333333,0.333333333333333,0.333333333333333,
0.333333333333333,0.333333333333333,0.333333333333333,0.333333333333333,
0.333333333333333,0.333333333333333,0.333333333333333,0.333333333333333,
0.333333333333333,0.333333333333333,0.333333333333333,0.333333333333333,
0.333333333333333,0.333333333333333,0.333333333333333,0.333333333333333,
0.333333333333333,0.333333333333333,0.333333333333333,0.333333333333333,
0.333333333333333,0.333333333333333,0.333333333333333,0.333333333333333,
0.333333333333333,0.333333333333333,0.333333333333333,0.333333333333333,
0.333333333333333,0.333333333333333,0.333333333333333,0.333333333333333,
0.333333333333333,0.333333333333333,0.333333333333333,0.333333333333333,
0.333333333333333,0.333333333333333,0.333333333333333),(0.333333333333333,
0.333333333333333,0.333333333333333,0.333333333333333,0.333333333333333,
0.333333333333333,0.333333333333333,0.333333333333333,0.333333333333333,
0.333333333333333,0.333333333333333,0.333333333333333,0.333333333333333,
0.333333333333333,0.333333333333333,0.333333333333333,0.333333333333333,
0.333333333333333,0.333333333333333,0.333333333333333,0.333333333333333,
0.333333333333333,0.333333333333333,0.333333333333333,0.333333333333333,
0.333333333333333,0.333333333333333,0.333333333333333,0.333333333333333,
0.333333333333333,0.333333333333333,0.333333333333333,0.333333333333333,
0.333333333333333,0.333333333333333,0.333333333333333,0.333333333333333,
0.333333333333333,0.333333333333333,0.333333333333333,0.333333333333333,
0.333333333333333,0.333333333333333,0.333333333333333,0.333333333333333,
0.333333333333333,0.333333333333333,0.333333333333333,0.333333333333333,
0.333333333333333,0.333333333333333,0.333333333333333,0.333333333333333,
0.333333333333333,0.333333333333333,0.333333333333333,0.333333333333333,
0.333333333333333,0.333333333333333,0.333333333333333,0.333333333333333,
0.333333333333333,0.333333333333333,0.333333333333333,0.333333333333333,
0.333333333333333,0.333333333333333,0.333333333333333,0.333333333333333,
0.333333333333333,0.333333333333333,0.333333333333333,0.333333333333333,
0.333333333333333,0.333333333333333,0.333333333333333,0.333333333333333,
0.333333333333333,0.333333333333333,0.333333333333333,0.333333333333333,
0.333333333333333,0.333333333333333,0.333333333333333,0.333333333333333,
0.333333333333333,0.333333333333333,0.333333333333333,0.333333333333333,
0.333333333333333,0.333333333333333,0.333333333333333,0.333333333333333,
0.333333333333333,0.333333333333333,0.333333333333333,0.333333333333333,
0.333333333333333,0.333333333333333,0.333333333333333,0.333333333333333,
0.333333333333333,0.333333333333333,0.333333333333333,0.333333333333333,
0.333333333333333,0.333333333333333,0.333333333333333,0.333333333333333,
0.333333333333333,0.333333333333333,0.333333333333333,0.333333333333333,
0.333333333333333,0.333333333333333,0.333333333333333,0.333333333333333,
0.333333333333333,0.333333333333333,0.333333333333333,0.333333333333333,
0.333333333333333,0.333333333333333,0.333333333333333,0.333333333333333,
0.333333333333333,0.333333333333333,0.333333333333333,0.333333333333333,
0.333333333333333),(1.,1.,1.,1.,1.,1.,1.,1.,1.,1.,1.,1.,1.,1.,1.,1.,1.,
1.,1.,1.,1.,1.,1.,1.,1.,1.,1.,1.,1.,1.,1.,1.,1.,1.,1.,1.,1.,1.,1.,1.,1.,
1.,1.,1.,1.,1.,1.,1.,1.,1.,1.,1.,1.,1.,1.,1.,1.,1.,1.,1.,1.,1.,1.,1.,1.,
1.,1.,1.,1.,1.,1.,1.,1.,1.,1.,1.,1.,1.,1.,1.,1.,1.,1.,1.,1.,1.,1.,1.,1.,
1.,1.,1.,1.,1.,1.,1.,1.,1.,1.,1.,1.,1.,1.,1.,1.,1.,1.,1.,1.,1.,1.,1.,1.,
1.,1.,1.,1.,1.,1.,1.,1.,1.,1.,1.,1.,1.,1.,1.,1.,1.)))
REPRESENTATION_ITEM('')
SURFACE()
);
#49=ELLIPSE('',#4023,0.175430953951623,0.175001932698577);
#50=SPHERICAL_SURFACE('',#3737,2.525);
#51=SPHERICAL_SURFACE('',#3742,6.);
#52=SPHERICAL_SURFACE('',#3746,6.);
#53=SPHERICAL_SURFACE('',#3750,6.);
#54=SPHERICAL_SURFACE('',#3754,6.);
#55=SPHERICAL_SURFACE('',#3800,6.);
#56=SPHERICAL_SURFACE('',#3803,6.);
#57=SPHERICAL_SURFACE('',#3807,6.);
#58=SPHERICAL_SURFACE('',#3811,6.);
#59=SPHERICAL_SURFACE('',#3814,6.);
#60=SPHERICAL_SURFACE('',#3817,6.);
#61=SPHERICAL_SURFACE('',#3821,6.);
#62=SPHERICAL_SURFACE('',#3825,6.);
#63=SPHERICAL_SURFACE('',#3829,0.05);
#64=SPHERICAL_SURFACE('',#3845,0.05);
#65=SPHERICAL_SURFACE('',#3847,0.05);
#66=SPHERICAL_SURFACE('',#3849,0.05);
#67=SPHERICAL_SURFACE('',#3851,0.05);
#68=SPHERICAL_SURFACE('',#3873,0.05);
#69=SPHERICAL_SURFACE('',#3875,0.05);
#70=SPHERICAL_SURFACE('',#3877,0.05);
#71=SPHERICAL_SURFACE('',#3879,0.05);
#72=SPHERICAL_SURFACE('',#3881,0.05);
#73=SPHERICAL_SURFACE('',#3883,0.05);
#74=SPHERICAL_SURFACE('',#3903,0.05);
#75=SPHERICAL_SURFACE('',#3905,0.05);
#76=SPHERICAL_SURFACE('',#3907,0.05);
#77=SPHERICAL_SURFACE('',#3909,0.05);
#78=SPHERICAL_SURFACE('',#3911,0.05);
#79=SPHERICAL_SURFACE('',#3913,0.05);
#80=SPHERICAL_SURFACE('',#3936,0.05);
#81=SPHERICAL_SURFACE('',#3938,0.05);
#82=SPHERICAL_SURFACE('',#3941,0.05);
#83=SPHERICAL_SURFACE('',#3943,0.05);
#84=SPHERICAL_SURFACE('',#3945,0.05);
#85=SPHERICAL_SURFACE('',#3946,0.05);
#86=SPHERICAL_SURFACE('',#3948,0.05);
#87=SPHERICAL_SURFACE('',#3968,0.05);
#88=SPHERICAL_SURFACE('',#3970,0.05);
#89=SPHERICAL_SURFACE('',#3972,0.05);
#90=SPHERICAL_SURFACE('',#3974,0.05);
#91=SPHERICAL_SURFACE('',#3990,0.05);
#92=SPHERICAL_SURFACE('',#3992,0.05);
#93=SPHERICAL_SURFACE('',#3994,0.05);
#94=SPHERICAL_SURFACE('',#3996,0.05);
#95=SPHERICAL_SURFACE('',#4006,0.05);
#96=SPHERICAL_SURFACE('',#4008,0.05);
#97=TOROIDAL_SURFACE('',#3724,2.70416345659799,0.05);
#98=TOROIDAL_SURFACE('',#3732,2.70416345659799,0.05);
#99=TOROIDAL_SURFACE('',#3835,2.70416345659799,0.05);
#100=TOROIDAL_SURFACE('',#3837,5.32728824074688,0.05);
#101=TOROIDAL_SURFACE('',#3840,5.32728824074688,0.05);
#102=TOROIDAL_SURFACE('',#3842,5.32728824074688,0.05);
#103=TOROIDAL_SURFACE('',#3854,5.32728824074688,0.05);
#104=TOROIDAL_SURFACE('',#3856,2.70416345659799,0.05);
#105=TOROIDAL_SURFACE('',#3862,5.32728824074688,0.05);
#106=TOROIDAL_SURFACE('',#3868,5.32728824074688,0.05);
#107=TOROIDAL_SURFACE('',#3887,5.32728824074688,0.05);
#108=TOROIDAL_SURFACE('',#3890,5.32728824074688,0.05);
#109=TOROIDAL_SURFACE('',#3892,5.32728824074688,0.05);
#110=TOROIDAL_SURFACE('',#3894,2.70416345659799,0.05);
#111=TOROIDAL_SURFACE('',#3896,2.70416345659799,0.05);
#112=TOROIDAL_SURFACE('',#3898,5.32728824074688,0.05);
#113=TOROIDAL_SURFACE('',#3900,5.32728824074688,0.05);
#114=TOROIDAL_SURFACE('',#3915,5.32728824074688,0.05);
#115=TOROIDAL_SURFACE('',#3917,2.70416345659799,0.05);
#116=TOROIDAL_SURFACE('',#3919,2.70416345659799,0.05);
#117=TOROIDAL_SURFACE('',#3926,5.32728824074688,0.05);
#118=TOROIDAL_SURFACE('',#3933,5.32728824074688,0.05);
#119=TOROIDAL_SURFACE('',#3954,5.32728824074688,0.05);
#120=TOROIDAL_SURFACE('',#3956,5.32728824074688,0.05);
#121=TOROIDAL_SURFACE('',#3958,5.32728824074688,0.05);
#122=TOROIDAL_SURFACE('',#3960,2.70416345659799,0.05);
#123=TOROIDAL_SURFACE('',#3962,5.32728824074688,0.05);
#124=TOROIDAL_SURFACE('',#3964,5.32728824074688,0.05);
#125=TOROIDAL_SURFACE('',#3966,5.32728824074688,0.05);
#126=TOROIDAL_SURFACE('',#3978,5.32728824074688,0.05);
#127=TOROIDAL_SURFACE('',#3985,5.32728824074688,0.05);
#128=TOROIDAL_SURFACE('',#3998,5.32728824074688,0.05);
#129=TOROIDAL_SURFACE('',#4000,2.70416345659799,0.05);
#130=TOROIDAL_SURFACE('',#4002,2.70416345659799,0.05);
#131=TOROIDAL_SURFACE('',#4004,5.32728824074688,0.05);
#132=TOROIDAL_SURFACE('',#4013,2.5,1.);
#133=TOROIDAL_SURFACE('',#4017,5.55,0.175);
#134=TOROIDAL_SURFACE('',#4020,3.17573472959676,0.175);
#135=CONICAL_SURFACE('',#3666,1.14999999999999,0.785398163397463);
#136=CONICAL_SURFACE('',#3674,1.99999999999999,0.0977269073587189);
#137=CONICAL_SURFACE('',#3719,1.15,0.785398163397453);
#138=B_SPLINE_CURVE_WITH_KNOTS('',3,(#6086,#6087,#6088,#6089,#6090,#6091,
#6092,#6093,#6094,#6095,#6096,#6097,#6098,#6099,#6100,#6101,#6102,#6103,
#6104,#6105,#6106,#6107),.UNSPECIFIED.,.F.,.F.,(4,2,2,2,2,2,2,2,2,2,4),
(-0.398476386723121,-0.363413449903791,-0.328945780906488,-0.279734113540581,
-0.238759142767186,-0.202537073889496,-0.166278974820396,-0.125546922866738,
-0.0748109574930432,-0.0377065280884949,0.),.UNSPECIFIED.);
#139=B_SPLINE_CURVE_WITH_KNOTS('',3,(#6111,#6112,#6113,#6114),
 .UNSPECIFIED.,.F.,.F.,(4,4),(-0.320868204557424,-0.320859930375376),
 .UNSPECIFIED.);
#140=B_SPLINE_CURVE_WITH_KNOTS('',3,(#6116,#6117,#6118,#6119,#6120,#6121,
#6122,#6123,#6124,#6125,#6126,#6127,#6128,#6129,#6130,#6131,#6132,#6133,
#6134,#6135,#6136,#6137,#6138,#6139),.UNSPECIFIED.,.F.,.F.,(4,2,2,2,2,2,
2,2,2,2,2,4),(-0.320859930375376,-0.303821997926792,-0.286725131861031,
-0.252375001979002,-0.231369369238555,-0.194211321091721,-0.160393271457449,
-0.126524952102273,-0.0894197007003378,-0.0475320396288663,-0.0237192939459634,
-1.00000035202497E-6),.UNSPECIFIED.);
#141=B_SPLINE_CURVE_WITH_KNOTS('',3,(#6635,#6636,#6637,#6638,#6639,#6640,
#6641,#6642,#6643,#6644,#6645,#6646,#6647,#6648,#6649,#6650,#6651,#6652,
#6653,#6654,#6655,#6656),.UNSPECIFIED.,.F.,.F.,(4,2,2,2,2,2,2,2,2,2,4),
(-0.398476386717938,-0.363413449898109,-0.328945780900276,-0.279734113534564,
-0.238759142762232,-0.202537073885482,-0.166278974817291,-0.125546922864936,
-0.074810957492591,-0.0377065280884339,0.),.UNSPECIFIED.);
#142=B_SPLINE_CURVE_WITH_KNOTS('',3,(#6660,#6661,#6662,#6663),
 .UNSPECIFIED.,.F.,.F.,(4,4),(-0.320868204532271,-0.320859930350223),
 .UNSPECIFIED.);
#143=B_SPLINE_CURVE_WITH_KNOTS('',3,(#6665,#6666,#6667,#6668,#6669,#6670,
#6671,#6672,#6673,#6674,#6675,#6676,#6677,#6678,#6679,#6680,#6681,#6682,
#6683,#6684,#6685,#6686,#6687,#6688),.UNSPECIFIED.,.F.,.F.,(4,2,2,2,2,2,
2,2,2,2,2,4),(-0.320859930350223,-0.303821997902903,-0.286725131838533,
-0.252375001959359,-0.23136936922067,-0.194211321076927,-0.160393271445428,
-0.126524952093029,-0.0894197006941437,-0.0475320396261598,-0.0237192939451105,
-1.00000035191394E-6),.UNSPECIFIED.);
#144=B_SPLINE_CURVE_WITH_KNOTS('',3,(#6712,#6713,#6714,#6715,#6716,#6717,
#6718,#6719,#6720,#6721,#6722,#6723,#6724,#6725,#6726,#6727,#6728,#6729,
#6730,#6731,#6732,#6733),.UNSPECIFIED.,.F.,.F.,(4,2,2,2,2,2,2,2,2,2,4),
(-0.420674421775538,-0.382950410823496,-0.345914295714904,-0.296541537335382,
-0.257099730998724,-0.212666956872446,-0.167430581836075,-0.126839008921964,
-0.0765690827106126,-0.0387810619783508,0.),.UNSPECIFIED.);
#145=B_SPLINE_CURVE_WITH_KNOTS('',3,(#6734,#6735,#6736,#6737,#6738,#6739,
#6740,#6741,#6742,#6743,#6744,#6745,#6746,#6747,#6748,#6749,#6750,#6751,
#6752,#6753,#6754,#6755),.UNSPECIFIED.,.F.,.F.,(4,2,2,2,2,2,2,2,2,2,4),
(-0.420674421739622,-0.382950410793912,-0.345914295692047,-0.296541537321962,
-0.257099730993021,-0.212666956872502,-0.1674305818364,-0.126839008922401,
-0.0765690827112369,-0.0387810619787167,0.),.UNSPECIFIED.);
#146=B_SPLINE_CURVE_WITH_KNOTS('',3,(#6760,#6761,#6762,#6763,#6764,#6765,
#6766,#6767,#6768,#6769,#6770,#6771,#6772,#6773,#6774,#6775,#6776,#6777,
#6778,#6779,#6780,#6781),.UNSPECIFIED.,.F.,.F.,(4,2,2,2,2,2,2,2,2,2,4),
(1.00000051704647E-6,0.0346979268821443,0.0692680598480025,0.109244972085431,
0.144041383182867,0.160697846212527,0.177234449156828,0.212032576255554,
0.252099494752921,0.286510766916454,0.320844032281287),.UNSPECIFIED.);
#147=B_SPLINE_CURVE_WITH_KNOTS('',3,(#6786,#6787,#6788,#6789,#6790,#6791,
#6792,#6793,#6794,#6795,#6796,#6797,#6798,#6799,#6800,#6801,#6802,#6803,
#6804,#6805,#6806,#6807),.UNSPECIFIED.,.F.,.F.,(4,2,2,2,2,2,2,2,2,2,4),
(1.00000051707666E-6,0.0346979268820894,0.0692680598476906,0.109244972084642,
0.14404138318175,0.160697846211195,0.17723444915527,0.212032576253597,0.252099494750475,
0.286510766913486,0.3208440322786),.UNSPECIFIED.);
#148=B_SPLINE_CURVE_WITH_KNOTS('',3,(#8129,#8130,#8131,#8132,#8133,#8134,
#8135,#8136,#8137,#8138,#8139,#8140),.UNSPECIFIED.,.F.,.F.,(4,2,2,2,2,4),
(0.0241248766269512,0.0242510021276225,0.0244868094400705,0.0259331295349885,
0.0273794496299066,0.0302720898197427),.UNSPECIFIED.);
#149=B_SPLINE_CURVE_WITH_KNOTS('',3,(#8142,#8143,#8144,#8145,#8146,#8147,
#8148,#8149,#8150,#8151,#8152,#8153),.UNSPECIFIED.,.F.,.F.,(4,2,2,2,2,4),
(0.103445236849632,0.106337877040163,0.107784197135428,0.109230517230693,
0.109466324543198,0.109592450043899),.UNSPECIFIED.);
#150=B_SPLINE_CURVE_WITH_KNOTS('',3,(#8379,#8380,#8381,#8382,#8383,#8384,
#8385,#8386),.UNSPECIFIED.,.F.,.F.,(4,2,2,4),(-0.000183878052419735,0.,
0.00168136886964635,0.00357997544050363),.UNSPECIFIED.);
#151=B_SPLINE_CURVE_WITH_KNOTS('',3,(#8388,#8389,#8390,#8391,#8392,#8393,
#8394,#8395,#8396,#8397,#8398,#8399,#8400,#8401,#8402,#8403,#8404,#8405,
#8406,#8407,#8408,#8409,#8410,#8411,#8412,#8413,#8414,#8415,#8416,#8417,
#8418,#8419,#8420,#8421,#8422,#8423),.UNSPECIFIED.,.F.,.F.,(4,2,2,2,2,2,
2,2,2,2,2,2,2,2,2,2,2,4),(-0.574674927918272,-0.571952286676393,-0.508824986264653,
-0.441235232795549,-0.327513816563257,-0.270706788955357,-0.257131961119942,
-0.253114953696847,-0.25068545375721,-0.248656048688706,-0.24640797600825,
-0.242733690405177,-0.23450108496833,-0.210223290532083,-0.0958268045063037,
-0.0460408693976727,-0.0223119527990917,-9.99999999917733E-7),
 .UNSPECIFIED.);
#152=B_SPLINE_CURVE_WITH_KNOTS('',3,(#8425,#8426,#8427,#8428,#8429,#8430,
#8431,#8432,#8433,#8434),.UNSPECIFIED.,.F.,.F.,(4,3,3,4),(0.00457726855862458,
0.00480753339462812,0.0050279498472682,0.00507749417619398),
 .UNSPECIFIED.);
#153=B_SPLINE_CURVE_WITH_KNOTS('',3,(#9347,#9348,#9349,#9350,#9351,#9352,
#9353,#9354,#9355,#9356,#9357,#9358,#9359,#9360,#9361,#9362,#9363,#9364,
#9365,#9366,#9367,#9368,#9369,#9370,#9371,#9372,#9373,#9374,#9375,#9376,
#9377,#9378,#9379,#9380,#9381,#9382,#9383,#9384,#9385,#9386,#9387,#9388,
#9389,#9390,#9391,#9392,#9393,#9394,#9395,#9396,#9397,#9398,#9399,#9400,
#9401,#9402,#9403,#9404,#9405,#9406,#9407,#9408,#9409,#9410,#9411,#9412,
#9413,#9414,#9415,#9416,#9417,#9418,#9419,#9420,#9421,#9422,#9423,#9424,
#9425,#9426,#9427,#9428,#9429,#9430,#9431,#9432,#9433,#9434,#9435,#9436,
#9437,#9438,#9439,#9440,#9441,#9442,#9443,#9444,#9445,#9446,#9447,#9448,
#9449,#9450,#9451,#9452,#9453,#9454,#9455,#9456,#9457,#9458,#9459,#9460,
#9461,#9462,#9463,#9464,#9465,#9466,#9467,#9468,#9469,#9470,#9471,#9472,
#9473,#9474,#9475,#9476),.UNSPECIFIED.,.F.,.F.,(4,2,2,2,2,2,2,2,2,2,2,2,
2,2,2,2,2,2,2,2,2,2,2,2,2,2,2,2,2,2,2,2,2,2,2,2,2,2,2,2,2,2,2,2,2,2,2,2,
2,2,2,2,2,2,2,2,2,2,2,2,2,2,2,2,4),(0.00652527768169836,0.015625,0.03125,
0.046875,0.0625,0.078125,0.09375,0.109375,0.125,0.140625,0.15625,0.171875,
0.1875,0.203125,0.21875,0.234375,0.25,0.265625,0.28125,0.296875,0.3125,
0.328125,0.34375,0.359375,0.375,0.390625,0.40625,0.421875,0.4375,0.453125,
0.46875,0.484375,0.5,0.515625,0.53125,0.546875,0.5625,0.578125,0.59375,
0.609375,0.625,0.640625,0.65625,0.671875,0.6875,0.703125,0.71875,0.734375,
0.75,0.765625,0.78125,0.796875,0.8125,0.828125,0.84375,0.859375,0.875,0.890625,
0.90625,0.921875,0.9375,0.953125,0.96875,0.984375,1.),.UNSPECIFIED.);
#154=B_SPLINE_CURVE_WITH_KNOTS('',3,(#9479,#9480,#9481,#9482,#9483,#9484,
#9485,#9486,#9487,#9488,#9489,#9490,#9491,#9492,#9493,#9494,#9495,#9496,
#9497,#9498,#9499,#9500,#9501,#9502,#9503,#9504,#9505,#9506,#9507,#9508,
#9509,#9510,#9511,#9512,#9513,#9514,#9515,#9516,#9517,#9518,#9519,#9520,
#9521,#9522,#9523,#9524,#9525,#9526,#9527,#9528,#9529,#9530,#9531,#9532,
#9533,#9534,#9535,#9536,#9537,#9538,#9539,#9540,#9541,#9542,#9543,#9544,
#9545,#9546,#9547,#9548,#9549,#9550,#9551,#9552,#9553,#9554,#9555,#9556,
#9557,#9558,#9559,#9560,#9561,#9562,#9563,#9564,#9565,#9566,#9567,#9568,
#9569,#9570,#9571,#9572,#9573,#9574,#9575,#9576,#9577,#9578,#9579,#9580,
#9581,#9582,#9583,#9584,#9585,#9586,#9587,#9588,#9589,#9590,#9591,#9592,
#9593,#9594,#9595,#9596,#9597,#9598,#9599,#9600,#9601,#9602,#9603,#9604,
#9605,#9606,#9607,#9608),.UNSPECIFIED.,.F.,.F.,(4,2,2,2,2,2,2,2,2,2,2,2,
2,2,2,2,2,2,2,2,2,2,2,2,2,2,2,2,2,2,2,2,2,2,2,2,2,2,2,2,2,2,2,2,2,2,2,2,
2,2,2,2,2,2,2,2,2,2,2,2,2,2,2,2,4),(3.07557452178047E-5,0.015625,0.03125,
0.046875,0.0625,0.078125,0.09375,0.109375,0.125,0.140625,0.15625,0.171875,
0.1875,0.203125,0.21875,0.234375,0.25,0.265625,0.28125,0.296875,0.3125,
0.328125,0.34375,0.359375,0.375,0.390625,0.40625,0.421875,0.4375,0.453125,
0.46875,0.484375,0.5,0.515625,0.53125,0.546875,0.5625,0.578125,0.59375,
0.609375,0.625,0.640625,0.65625,0.671875,0.6875,0.703125,0.71875,0.734375,
0.75,0.765625,0.78125,0.796875,0.8125,0.828125,0.84375,0.859375,0.875,0.890625,
0.90625,0.921875,0.9375,0.953125,0.96875,0.984375,1.),.UNSPECIFIED.);
#155=B_SPLINE_SURFACE_WITH_KNOTS('',1,3,((#5592,#5593,#5594,#5595,#5596,
#5597,#5598,#5599,#5600,#5601,#5602,#5603,#5604,#5605,#5606,#5607,#5608,
#5609,#5610,#5611,#5612,#5613,#5614,#5615,#5616,#5617,#5618,#5619,#5620,
#5621,#5622,#5623,#5624,#5625,#5626,#5627,#5628,#5629,#5630,#5631,#5632,
#5633,#5634,#5635,#5636,#5637,#5638,#5639,#5640,#5641,#5642,#5643,#5644,
#5645,#5646,#5647,#5648,#5649,#5650,#5651,#5652,#5653,#5654,#5655,#5656,
#5657,#5658,#5659,#5660,#5661,#5662,#5663,#5664,#5665,#5666,#5667,#5668,
#5669,#5670,#5671,#5672,#5673,#5674,#5675,#5676,#5677,#5678,#5679,#5680,
#5681,#5682,#5683,#5684,#5685,#5686,#5687,#5688,#5689,#5690,#5691,#5692,
#5693,#5694,#5695,#5696,#5697,#5698,#5699,#5700,#5701,#5702,#5703,#5704,
#5705,#5706,#5707,#5708,#5709,#5710,#5711,#5712,#5713,#5714,#5715,#5716,
#5717,#5718,#5719,#5720,#5721,#5722,#5723,#5724,#5725,#5726,#5727,#5728,
#5729,#5730,#5731,#5732,#5733,#5734,#5735,#5736,#5737,#5738,#5739,#5740,
#5741,#5742,#5743,#5744,#5745,#5746,#5747,#5748,#5749,#5750,#5751,#5752,
#5753,#5754,#5755,#5756,#5757,#5758,#5759,#5760,#5761,#5762,#5763,#5764,
#5765,#5766,#5767,#5768,#5769,#5770,#5771,#5772,#5773,#5774,#5775,#5776,
#5777,#5778,#5779,#5780,#5781,#5782,#5783,#5784,#5785,#5786,#5787,#5788,
#5789,#5790,#5791,#5792,#5793,#5794,#5795,#5796,#5797,#5798,#5799,#5800,
#5801,#5802,#5803,#5804,#5805,#5806,#5807,#5808,#5809,#5810,#5811,#5812,
#5813,#5814,#5815,#5816,#5817,#5818,#5819,#5820,#5821,#5822,#5823,#5824,
#5825,#5826,#5827,#5828,#5829,#5830,#5831,#5832,#5833,#5834,#5835,#5836,
#5837),(#5838,#5839,#5840,#5841,#5842,#5843,#5844,#5845,#5846,#5847,#5848,
#5849,#5850,#5851,#5852,#5853,#5854,#5855,#5856,#5857,#5858,#5859,#5860,
#5861,#5862,#5863,#5864,#5865,#5866,#5867,#5868,#5869,#5870,#5871,#5872,
#5873,#5874,#5875,#5876,#5877,#5878,#5879,#5880,#5881,#5882,#5883,#5884,
#5885,#5886,#5887,#5888,#5889,#5890,#5891,#5892,#5893,#5894,#5895,#5896,
#5897,#5898,#5899,#5900,#5901,#5902,#5903,#5904,#5905,#5906,#5907,#5908,
#5909,#5910,#5911,#5912,#5913,#5914,#5915,#5916,#5917,#5918,#5919,#5920,
#5921,#5922,#5923,#5924,#5925,#5926,#5927,#5928,#5929,#5930,#5931,#5932,
#5933,#5934,#5935,#5936,#5937,#5938,#5939,#5940,#5941,#5942,#5943,#5944,
#5945,#5946,#5947,#5948,#5949,#5950,#5951,#5952,#5953,#5954,#5955,#5956,
#5957,#5958,#5959,#5960,#5961,#5962,#5963,#5964,#5965,#5966,#5967,#5968,
#5969,#5970,#5971,#5972,#5973,#5974,#5975,#5976,#5977,#5978,#5979,#5980,
#5981,#5982,#5983,#5984,#5985,#5986,#5987,#5988,#5989,#5990,#5991,#5992,
#5993,#5994,#5995,#5996,#5997,#5998,#5999,#6000,#6001,#6002,#6003,#6004,
#6005,#6006,#6007,#6008,#6009,#6010,#6011,#6012,#6013,#6014,#6015,#6016,
#6017,#6018,#6019,#6020,#6021,#6022,#6023,#6024,#6025,#6026,#6027,#6028,
#6029,#6030,#6031,#6032,#6033,#6034,#6035,#6036,#6037,#6038,#6039,#6040,
#6041,#6042,#6043,#6044,#6045,#6046,#6047,#6048,#6049,#6050,#6051,#6052,
#6053,#6054,#6055,#6056,#6057,#6058,#6059,#6060,#6061,#6062,#6063,#6064,
#6065,#6066,#6067,#6068,#6069,#6070,#6071,#6072,#6073,#6074,#6075,#6076,
#6077,#6078,#6079,#6080,#6081,#6082,#6083)),.UNSPECIFIED.,.F.,.T.,.F.,(2,
2),(4,2,2,2,2,2,2,2,2,2,2,2,2,2,2,2,2,2,2,2,2,2,2,2,2,2,2,2,2,2,2,2,2,2,
2,2,2,2,2,2,2,2,2,2,2,2,2,2,2,2,2,2,2,2,2,2,2,2,2,2,2,2,2,2,2,2,2,2,2,2,
2,2,2,2,2,2,2,2,2,2,2,2,2,2,2,2,2,2,2,2,2,2,2,2,2,2,2,2,2,2,2,2,2,2,2,2,
2,2,2,2,2,2,2,2,2,2,2,2,2,2,2,2,4),(-1.00016962386399E-6,1.),(0.000438425814883596,
0.00049639971234602,0.000554373609808444,0.000670321404733293,0.000728295302195718,
0.00075728225092693,0.000786269199658142,0.000844243097120567,0.000902216994582991,
0.00101816478950784,0.00107613868697026,0.00113411258443269,0.00119208648189511,
0.00125006037935754,0.00136600817428239,0.00142398207174481,0.00148195596920724,
0.00153992986666966,0.00159790376413208,0.00165587766159451,0.00171385155905693,
0.00182979935398178,0.00188777325144421,0.00191676020017542,0.00194574714890663,
0.00200372104636906,0.00206169494383148,0.00217764273875633,0.00223561663621875,
0.00229359053368118,0.0023515644311436,0.00240953832860603,0.00246751222606845,
0.00252548612353088,0.00264143391845572,0.00267042086718694,0.00269940781591815,
0.00275738171338057,0.002815355610843,0.00287332950830542,0.00293130340576785,
0.00298927730323027,0.0030472512006927,0.00310522509815512,0.00316319899561754,
0.00322117289307997,0.00333712068800482,0.00339509458546724,0.00342408153419845,
0.00345306848292967,0.00351104238039209,0.00356901627785452,0.00368496407277936,
0.00380091186770421,0.00385888576516664,0.00391685966262906,0.00397483356009149,
0.00403280745755391,0.00414875525247876,0.00420672914994119,0.00426470304740361,
0.00432267694486603,0.00438065084232846,0.00443862473979088,0.00449659863725331,
0.00461254643217816,0.00467052032964058,0.00469950727837179,0.00472849422710301,
0.00478646812456543,0.00484444202202785,0.0049603898169527,0.00501836371441513,
0.00507633761187755,0.00510532456060876,0.00513431150933998,0.0051922854068024,
0.00530823320172725,0.00536620709918968,0.0054241809966521,0.00548215489411452,
0.00551114184284574,0.00554012879157695,0.0056560765865018,0.00577202438142665,
0.00582999827888907,0.00588797217635149,0.00591695912508271,0.00594594607381392,
0.00600391997127634,0.00611986776620119,0.00617784166366362,0.00623581556112604,
0.00626480250985725,0.00629378945858847,0.00635176335605089,0.00640973725351331,
0.00646771115097574,0.00658365894590059,0.0066126458946318,0.00664163284336301,
0.00669960674082544,0.00675758063828786,0.00681555453575028,0.00687352843321271,
0.00693150233067513,0.00698947622813756,0.00701846317686877,0.00704745012559998,
0.00716339792052483,0.00727934571544968,0.0073373196129121,0.00739529351037453,
0.00742428045910574,0.00745326740783695,0.00751124130529938,0.0075692152027618,
0.00762718910022423,0.00768516299768665,0.00774313689514908,0.0078011107926115,
0.00783009774134271,0.00785908469007393),.UNSPECIFIED.);
#156=B_SPLINE_SURFACE_WITH_KNOTS('',1,3,((#6141,#6142,#6143,#6144,#6145,
#6146,#6147,#6148,#6149,#6150,#6151,#6152,#6153,#6154,#6155,#6156,#6157,
#6158,#6159,#6160,#6161,#6162,#6163,#6164,#6165,#6166,#6167,#6168,#6169,
#6170,#6171,#6172,#6173,#6174,#6175,#6176,#6177,#6178,#6179,#6180,#6181,
#6182,#6183,#6184,#6185,#6186,#6187,#6188,#6189,#6190,#6191,#6192,#6193,
#6194,#6195,#6196,#6197,#6198,#6199,#6200,#6201,#6202,#6203,#6204,#6205,
#6206,#6207,#6208,#6209,#6210,#6211,#6212,#6213,#6214,#6215,#6216,#6217,
#6218,#6219,#6220,#6221,#6222,#6223,#6224,#6225,#6226,#6227,#6228,#6229,
#6230,#6231,#6232,#6233,#6234,#6235,#6236,#6237,#6238,#6239,#6240,#6241,
#6242,#6243,#6244,#6245,#6246,#6247,#6248,#6249,#6250,#6251,#6252,#6253,
#6254,#6255,#6256,#6257,#6258,#6259,#6260,#6261,#6262,#6263,#6264,#6265,
#6266,#6267,#6268,#6269,#6270,#6271,#6272,#6273,#6274,#6275,#6276,#6277,
#6278,#6279,#6280,#6281,#6282,#6283,#6284,#6285,#6286,#6287,#6288,#6289,
#6290,#6291,#6292,#6293,#6294,#6295,#6296,#6297,#6298,#6299,#6300,#6301,
#6302,#6303,#6304,#6305,#6306,#6307,#6308,#6309,#6310,#6311,#6312,#6313,
#6314,#6315,#6316,#6317,#6318,#6319,#6320,#6321,#6322,#6323,#6324,#6325,
#6326,#6327,#6328,#6329,#6330,#6331,#6332,#6333,#6334,#6335,#6336,#6337,
#6338,#6339,#6340,#6341,#6342,#6343,#6344,#6345,#6346,#6347,#6348,#6349,
#6350,#6351,#6352,#6353,#6354,#6355,#6356,#6357,#6358,#6359,#6360,#6361,
#6362,#6363,#6364,#6365,#6366,#6367,#6368,#6369,#6370,#6371,#6372,#6373,
#6374,#6375,#6376,#6377,#6378,#6379,#6380,#6381,#6382,#6383,#6384,#6385,
#6386),(#6387,#6388,#6389,#6390,#6391,#6392,#6393,#6394,#6395,#6396,#6397,
#6398,#6399,#6400,#6401,#6402,#6403,#6404,#6405,#6406,#6407,#6408,#6409,
#6410,#6411,#6412,#6413,#6414,#6415,#6416,#6417,#6418,#6419,#6420,#6421,
#6422,#6423,#6424,#6425,#6426,#6427,#6428,#6429,#6430,#6431,#6432,#6433,
#6434,#6435,#6436,#6437,#6438,#6439,#6440,#6441,#6442,#6443,#6444,#6445,
#6446,#6447,#6448,#6449,#6450,#6451,#6452,#6453,#6454,#6455,#6456,#6457,
#6458,#6459,#6460,#6461,#6462,#6463,#6464,#6465,#6466,#6467,#6468,#6469,
#6470,#6471,#6472,#6473,#6474,#6475,#6476,#6477,#6478,#6479,#6480,#6481,
#6482,#6483,#6484,#6485,#6486,#6487,#6488,#6489,#6490,#6491,#6492,#6493,
#6494,#6495,#6496,#6497,#6498,#6499,#6500,#6501,#6502,#6503,#6504,#6505,
#6506,#6507,#6508,#6509,#6510,#6511,#6512,#6513,#6514,#6515,#6516,#6517,
#6518,#6519,#6520,#6521,#6522,#6523,#6524,#6525,#6526,#6527,#6528,#6529,
#6530,#6531,#6532,#6533,#6534,#6535,#6536,#6537,#6538,#6539,#6540,#6541,
#6542,#6543,#6544,#6545,#6546,#6547,#6548,#6549,#6550,#6551,#6552,#6553,
#6554,#6555,#6556,#6557,#6558,#6559,#6560,#6561,#6562,#6563,#6564,#6565,
#6566,#6567,#6568,#6569,#6570,#6571,#6572,#6573,#6574,#6575,#6576,#6577,
#6578,#6579,#6580,#6581,#6582,#6583,#6584,#6585,#6586,#6587,#6588,#6589,
#6590,#6591,#6592,#6593,#6594,#6595,#6596,#6597,#6598,#6599,#6600,#6601,
#6602,#6603,#6604,#6605,#6606,#6607,#6608,#6609,#6610,#6611,#6612,#6613,
#6614,#6615,#6616,#6617,#6618,#6619,#6620,#6621,#6622,#6623,#6624,#6625,
#6626,#6627,#6628,#6629,#6630,#6631,#6632)),.UNSPECIFIED.,.F.,.T.,.F.,(2,
2),(4,2,2,2,2,2,2,2,2,2,2,2,2,2,2,2,2,2,2,2,2,2,2,2,2,2,2,2,2,2,2,2,2,2,
2,2,2,2,2,2,2,2,2,2,2,2,2,2,2,2,2,2,2,2,2,2,2,2,2,2,2,2,2,2,2,2,2,2,2,2,
2,2,2,2,2,2,2,2,2,2,2,2,2,2,2,2,2,2,2,2,2,2,2,2,2,2,2,2,2,2,2,2,2,2,2,2,
2,2,2,2,2,2,2,2,2,2,2,2,2,2,2,2,4),(-1.00016962714665E-6,1.),(0.000438425814883592,
0.000496399712346016,0.000554373609808441,0.000670321404733289,0.000728295302195713,
0.000757282250926925,0.000786269199658137,0.000844243097120562,0.000902216994582986,
0.00101816478950783,0.00107613868697026,0.00113411258443268,0.00119208648189511,
0.00125006037935753,0.00136600817428238,0.0014239820717448,0.00148195596920723,
0.00153992986666965,0.00159790376413208,0.0016558776615945,0.00171385155905693,
0.00182979935398177,0.0018877732514442,0.00191676020017541,0.00194574714890662,
0.00200372104636905,0.00206169494383147,0.00217764273875632,0.00223561663621874,
0.00229359053368117,0.00235156443114359,0.00240953832860602,0.00246751222606844,
0.00252548612353086,0.00264143391845571,0.00267042086718692,0.00269940781591814,
0.00275738171338056,0.00281535561084298,0.00287332950830541,0.00293130340576783,
0.00298927730323026,0.00304725120069268,0.00310522509815511,0.00316319899561753,
0.00322117289307996,0.0033371206880048,0.00339509458546723,0.00342408153419844,
0.00345306848292965,0.00351104238039208,0.0035690162778545,0.00368496407277935,
0.0038009118677042,0.00385888576516662,0.00391685966262905,0.00397483356009147,
0.00403280745755389,0.00414875525247874,0.00420672914994117,0.00426470304740359,
0.00432267694486602,0.00438065084232844,0.00443862473979086,0.00449659863725329,
0.00461254643217814,0.00467052032964056,0.00469950727837177,0.00472849422710298,
0.00478646812456541,0.00484444202202783,0.00496038981695268,0.00501836371441511,
0.00507633761187753,0.00510532456060874,0.00513431150933995,0.00519228540680238,
0.00530823320172723,0.00536620709918965,0.00542418099665208,0.0054821548941145,
0.00551114184284571,0.00554012879157692,0.00565607658650177,0.00577202438142662,
0.00582999827888904,0.00588797217635147,0.00591695912508268,0.00594594607381389,
0.00600391997127632,0.00611986776620117,0.00617784166366359,0.00623581556112602,
0.00626480250985723,0.00629378945858844,0.00635176335605086,0.00640973725351329,
0.00646771115097571,0.00658365894590056,0.00661264589463177,0.00664163284336298,
0.00669960674082541,0.00675758063828783,0.00681555453575026,0.00687352843321268,
0.00693150233067511,0.00698947622813753,0.00701846317686874,0.00704745012559995,
0.0071633979205248,0.00727934571544965,0.00733731961291207,0.0073952935103745,
0.00742428045910571,0.00745326740783692,0.00751124130529935,0.00756921520276177,
0.0076271891002242,0.00768516299768662,0.00774313689514904,0.00780111079261147,
0.00783009774134268,0.00785908469007389),.UNSPECIFIED.);
#157=B_SPLINE_SURFACE_WITH_KNOTS('',1,3,((#6848,#6849,#6850,#6851,#6852,
#6853,#6854,#6855,#6856,#6857,#6858,#6859,#6860,#6861,#6862,#6863,#6864,
#6865,#6866,#6867,#6868,#6869,#6870,#6871,#6872,#6873,#6874,#6875,#6876,
#6877,#6878,#6879,#6880,#6881,#6882,#6883,#6884,#6885,#6886,#6887,#6888,
#6889,#6890,#6891,#6892,#6893,#6894,#6895,#6896,#6897,#6898,#6899,#6900,
#6901,#6902,#6903,#6904,#6905,#6906,#6907,#6908,#6909,#6910,#6911,#6912,
#6913,#6914,#6915,#6916,#6917,#6918,#6919,#6920,#6921,#6922,#6923,#6924,
#6925,#6926,#6927,#6928,#6929,#6930,#6931,#6932,#6933,#6934,#6935,#6936,
#6937,#6938,#6939,#6940,#6941,#6942,#6943,#6944,#6945,#6946,#6947,#6948,
#6949,#6950,#6951,#6952,#6953,#6954,#6955,#6956,#6957,#6958,#6959,#6960,
#6961,#6962,#6963,#6964,#6965,#6966,#6967,#6968,#6969,#6970,#6971,#6972,
#6973,#6974,#6975,#6976,#6977,#6978,#6979,#6980,#6981,#6982,#6983,#6984,
#6985,#6986,#6987,#6988,#6989,#6990,#6991,#6992,#6993,#6994,#6995,#6996,
#6997,#6998,#6999,#7000,#7001,#7002,#7003,#7004,#7005,#7006,#7007,#7008,
#7009,#7010,#7011,#7012,#7013,#7014,#7015,#7016,#7017,#7018,#7019,#7020,
#7021,#7022,#7023,#7024,#7025,#7026,#7027,#7028,#7029,#7030,#7031,#7032,
#7033,#7034,#7035,#7036,#7037,#7038,#7039,#7040,#7041,#7042,#7043,#7044,
#7045,#7046,#7047,#7048,#7049,#7050,#7051,#7052,#7053,#7054,#7055,#7056,
#7057,#7058,#7059,#7060,#7061,#7062,#7063,#7064,#7065,#7066,#7067,#7068,
#7069,#7070,#7071,#7072,#7073,#7074,#7075,#7076,#7077,#7078,#7079,#7080,
#7081,#7082,#7083,#7084,#7085,#7086,#7087,#7088,#7089,#7090,#7091,#7092,
#7093),(#7094,#7095,#7096,#7097,#7098,#7099,#7100,#7101,#7102,#7103,#7104,
#7105,#7106,#7107,#7108,#7109,#7110,#7111,#7112,#7113,#7114,#7115,#7116,
#7117,#7118,#7119,#7120,#7121,#7122,#7123,#7124,#7125,#7126,#7127,#7128,
#7129,#7130,#7131,#7132,#7133,#7134,#7135,#7136,#7137,#7138,#7139,#7140,
#7141,#7142,#7143,#7144,#7145,#7146,#7147,#7148,#7149,#7150,#7151,#7152,
#7153,#7154,#7155,#7156,#7157,#7158,#7159,#7160,#7161,#7162,#7163,#7164,
#7165,#7166,#7167,#7168,#7169,#7170,#7171,#7172,#7173,#7174,#7175,#7176,
#7177,#7178,#7179,#7180,#7181,#7182,#7183,#7184,#7185,#7186,#7187,#7188,
#7189,#7190,#7191,#7192,#7193,#7194,#7195,#7196,#7197,#7198,#7199,#7200,
#7201,#7202,#7203,#7204,#7205,#7206,#7207,#7208,#7209,#7210,#7211,#7212,
#7213,#7214,#7215,#7216,#7217,#7218,#7219,#7220,#7221,#7222,#7223,#7224,
#7225,#7226,#7227,#7228,#7229,#7230,#7231,#7232,#7233,#7234,#7235,#7236,
#7237,#7238,#7239,#7240,#7241,#7242,#7243,#7244,#7245,#7246,#7247,#7248,
#7249,#7250,#7251,#7252,#7253,#7254,#7255,#7256,#7257,#7258,#7259,#7260,
#7261,#7262,#7263,#7264,#7265,#7266,#7267,#7268,#7269,#7270,#7271,#7272,
#7273,#7274,#7275,#7276,#7277,#7278,#7279,#7280,#7281,#7282,#7283,#7284,
#7285,#7286,#7287,#7288,#7289,#7290,#7291,#7292,#7293,#7294,#7295,#7296,
#7297,#7298,#7299,#7300,#7301,#7302,#7303,#7304,#7305,#7306,#7307,#7308,
#7309,#7310,#7311,#7312,#7313,#7314,#7315,#7316,#7317,#7318,#7319,#7320,
#7321,#7322,#7323,#7324,#7325,#7326,#7327,#7328,#7329,#7330,#7331,#7332,
#7333,#7334,#7335,#7336,#7337,#7338,#7339)),.UNSPECIFIED.,.F.,.T.,.F.,(2,
2),(4,2,2,2,2,2,2,2,2,2,2,2,2,2,2,2,2,2,2,2,2,2,2,2,2,2,2,2,2,2,2,2,2,2,
2,2,2,2,2,2,2,2,2,2,2,2,2,2,2,2,2,2,2,2,2,2,2,2,2,2,2,2,2,2,2,2,2,2,2,2,
2,2,2,2,2,2,2,2,2,2,2,2,2,2,2,2,2,2,2,2,2,2,2,2,2,2,2,2,2,2,2,2,2,2,2,2,
2,2,2,2,2,2,2,2,2,2,2,2,2,2,2,2,4),(-3.16760819181413E-6,1.00000897992091),
(0.000438425814883592,0.000496399712346016,0.000554373609808441,0.000670321404733289,
0.000728295302195713,0.000757282250926925,0.000786269199658137,0.000844243097120562,
0.000902216994582986,0.00101816478950783,0.00107613868697026,0.00113411258443268,
0.00119208648189511,0.00125006037935753,0.00136600817428238,0.0014239820717448,
0.00148195596920723,0.00153992986666965,0.00159790376413208,0.0016558776615945,
0.00171385155905693,0.00182979935398177,0.0018877732514442,0.00191676020017541,
0.00194574714890662,0.00200372104636905,0.00206169494383147,0.00217764273875632,
0.00223561663621874,0.00229359053368117,0.00235156443114359,0.00240953832860602,
0.00246751222606844,0.00252548612353086,0.00264143391845571,0.00267042086718692,
0.00269940781591814,0.00275738171338056,0.00281535561084298,0.00287332950830541,
0.00293130340576783,0.00298927730323026,0.00304725120069268,0.00310522509815511,
0.00316319899561753,0.00322117289307996,0.0033371206880048,0.00339509458546723,
0.00342408153419844,0.00345306848292965,0.00351104238039208,0.0035690162778545,
0.00368496407277935,0.0038009118677042,0.00385888576516662,0.00391685966262905,
0.00397483356009147,0.00403280745755389,0.00414875525247874,0.00420672914994117,
0.00426470304740359,0.00432267694486602,0.00438065084232844,0.00443862473979086,
0.00449659863725329,0.00461254643217814,0.00467052032964056,0.00469950727837177,
0.00472849422710298,0.00478646812456541,0.00484444202202783,0.00496038981695268,
0.00501836371441511,0.00507633761187753,0.00510532456060874,0.00513431150933995,
0.00519228540680238,0.00530823320172723,0.00536620709918965,0.00542418099665208,
0.0054821548941145,0.00551114184284571,0.00554012879157692,0.00565607658650177,
0.00577202438142662,0.00582999827888904,0.00588797217635147,0.00591695912508268,
0.00594594607381389,0.00600391997127632,0.00611986776620117,0.00617784166366359,
0.00623581556112602,0.00626480250985723,0.00629378945858844,0.00635176335605086,
0.00640973725351329,0.00646771115097571,0.00658365894590056,0.00661264589463177,
0.00664163284336298,0.00669960674082541,0.00675758063828783,0.00681555453575026,
0.00687352843321268,0.00693150233067511,0.00698947622813753,0.00701846317686874,
0.00704745012559995,0.0071633979205248,0.00727934571544965,0.00733731961291207,
0.0073952935103745,0.00742428045910571,0.00745326740783692,0.00751124130529935,
0.00756921520276177,0.0076271891002242,0.00768516299768662,0.00774313689514904,
0.00780111079261147,0.00783009774134268,0.00785908469007389),
 .UNSPECIFIED.);
#158=B_SPLINE_SURFACE_WITH_KNOTS('',1,3,((#7340,#7341,#7342,#7343,#7344,
#7345,#7346,#7347,#7348,#7349,#7350,#7351,#7352,#7353,#7354,#7355,#7356,
#7357,#7358,#7359,#7360,#7361,#7362,#7363,#7364,#7365,#7366,#7367,#7368,
#7369,#7370,#7371,#7372,#7373,#7374,#7375,#7376,#7377,#7378,#7379,#7380,
#7381,#7382,#7383,#7384,#7385,#7386,#7387,#7388,#7389,#7390,#7391,#7392,
#7393,#7394,#7395,#7396,#7397,#7398,#7399,#7400,#7401,#7402,#7403,#7404,
#7405,#7406,#7407,#7408,#7409,#7410,#7411,#7412,#7413,#7414,#7415,#7416,
#7417,#7418,#7419,#7420,#7421,#7422,#7423,#7424,#7425,#7426,#7427,#7428,
#7429,#7430,#7431,#7432,#7433,#7434,#7435,#7436,#7437,#7438,#7439,#7440,
#7441,#7442,#7443,#7444,#7445,#7446,#7447,#7448,#7449,#7450,#7451,#7452,
#7453,#7454,#7455,#7456,#7457,#7458,#7459,#7460,#7461,#7462,#7463,#7464,
#7465,#7466,#7467,#7468,#7469,#7470,#7471,#7472,#7473,#7474,#7475,#7476,
#7477,#7478,#7479,#7480,#7481,#7482,#7483,#7484,#7485,#7486,#7487,#7488,
#7489,#7490,#7491,#7492,#7493,#7494,#7495,#7496,#7497,#7498,#7499,#7500,
#7501,#7502,#7503,#7504,#7505,#7506,#7507,#7508,#7509,#7510,#7511,#7512,
#7513,#7514,#7515,#7516,#7517,#7518,#7519,#7520,#7521,#7522,#7523,#7524,
#7525,#7526,#7527,#7528,#7529,#7530,#7531,#7532,#7533,#7534,#7535,#7536,
#7537,#7538,#7539,#7540,#7541,#7542,#7543,#7544,#7545,#7546,#7547,#7548,
#7549,#7550,#7551,#7552,#7553,#7554,#7555,#7556,#7557,#7558,#7559,#7560,
#7561,#7562,#7563,#7564,#7565,#7566,#7567,#7568,#7569,#7570,#7571,#7572,
#7573,#7574,#7575,#7576,#7577,#7578,#7579,#7580,#7581,#7582,#7583,#7584,
#7585),(#7586,#7587,#7588,#7589,#7590,#7591,#7592,#7593,#7594,#7595,#7596,
#7597,#7598,#7599,#7600,#7601,#7602,#7603,#7604,#7605,#7606,#7607,#7608,
#7609,#7610,#7611,#7612,#7613,#7614,#7615,#7616,#7617,#7618,#7619,#7620,
#7621,#7622,#7623,#7624,#7625,#7626,#7627,#7628,#7629,#7630,#7631,#7632,
#7633,#7634,#7635,#7636,#7637,#7638,#7639,#7640,#7641,#7642,#7643,#7644,
#7645,#7646,#7647,#7648,#7649,#7650,#7651,#7652,#7653,#7654,#7655,#7656,
#7657,#7658,#7659,#7660,#7661,#7662,#7663,#7664,#7665,#7666,#7667,#7668,
#7669,#7670,#7671,#7672,#7673,#7674,#7675,#7676,#7677,#7678,#7679,#7680,
#7681,#7682,#7683,#7684,#7685,#7686,#7687,#7688,#7689,#7690,#7691,#7692,
#7693,#7694,#7695,#7696,#7697,#7698,#7699,#7700,#7701,#7702,#7703,#7704,
#7705,#7706,#7707,#7708,#7709,#7710,#7711,#7712,#7713,#7714,#7715,#7716,
#7717,#7718,#7719,#7720,#7721,#7722,#7723,#7724,#7725,#7726,#7727,#7728,
#7729,#7730,#7731,#7732,#7733,#7734,#7735,#7736,#7737,#7738,#7739,#7740,
#7741,#7742,#7743,#7744,#7745,#7746,#7747,#7748,#7749,#7750,#7751,#7752,
#7753,#7754,#7755,#7756,#7757,#7758,#7759,#7760,#7761,#7762,#7763,#7764,
#7765,#7766,#7767,#7768,#7769,#7770,#7771,#7772,#7773,#7774,#7775,#7776,
#7777,#7778,#7779,#7780,#7781,#7782,#7783,#7784,#7785,#7786,#7787,#7788,
#7789,#7790,#7791,#7792,#7793,#7794,#7795,#7796,#7797,#7798,#7799,#7800,
#7801,#7802,#7803,#7804,#7805,#7806,#7807,#7808,#7809,#7810,#7811,#7812,
#7813,#7814,#7815,#7816,#7817,#7818,#7819,#7820,#7821,#7822,#7823,#7824,
#7825,#7826,#7827,#7828,#7829,#7830,#7831)),.UNSPECIFIED.,.F.,.T.,.F.,(2,
2),(4,2,2,2,2,2,2,2,2,2,2,2,2,2,2,2,2,2,2,2,2,2,2,2,2,2,2,2,2,2,2,2,2,2,
2,2,2,2,2,2,2,2,2,2,2,2,2,2,2,2,2,2,2,2,2,2,2,2,2,2,2,2,2,2,2,2,2,2,2,2,
2,2,2,2,2,2,2,2,2,2,2,2,2,2,2,2,2,2,2,2,2,2,2,2,2,2,2,2,2,2,2,2,2,2,2,2,
2,2,2,2,2,2,2,2,2,2,2,2,2,2,2,2,4),(-3.16760819184598E-6,1.00000897992087),
(0.000438425814883596,0.00049639971234602,0.000554373609808444,0.000670321404733293,
0.000728295302195718,0.00075728225092693,0.000786269199658142,0.000844243097120567,
0.000902216994582991,0.00101816478950784,0.00107613868697026,0.00113411258443269,
0.00119208648189511,0.00125006037935754,0.00136600817428239,0.00142398207174481,
0.00148195596920724,0.00153992986666966,0.00159790376413208,0.00165587766159451,
0.00171385155905693,0.00182979935398178,0.00188777325144421,0.00191676020017542,
0.00194574714890663,0.00200372104636906,0.00206169494383148,0.00217764273875633,
0.00223561663621875,0.00229359053368118,0.0023515644311436,0.00240953832860603,
0.00246751222606845,0.00252548612353088,0.00264143391845572,0.00267042086718694,
0.00269940781591815,0.00275738171338057,0.002815355610843,0.00287332950830542,
0.00293130340576785,0.00298927730323027,0.0030472512006927,0.00310522509815512,
0.00316319899561754,0.00322117289307997,0.00333712068800482,0.00339509458546724,
0.00342408153419845,0.00345306848292967,0.00351104238039209,0.00356901627785452,
0.00368496407277936,0.00380091186770421,0.00385888576516664,0.00391685966262906,
0.00397483356009149,0.00403280745755391,0.00414875525247876,0.00420672914994119,
0.00426470304740361,0.00432267694486603,0.00438065084232846,0.00443862473979088,
0.00449659863725331,0.00461254643217816,0.00467052032964058,0.00469950727837179,
0.00472849422710301,0.00478646812456543,0.00484444202202785,0.0049603898169527,
0.00501836371441513,0.00507633761187755,0.00510532456060876,0.00513431150933998,
0.0051922854068024,0.00530823320172725,0.00536620709918968,0.0054241809966521,
0.00548215489411452,0.00551114184284574,0.00554012879157695,0.0056560765865018,
0.00577202438142665,0.00582999827888907,0.00588797217635149,0.00591695912508271,
0.00594594607381392,0.00600391997127634,0.00611986776620119,0.00617784166366362,
0.00623581556112604,0.00626480250985725,0.00629378945858847,0.00635176335605089,
0.00640973725351331,0.00646771115097574,0.00658365894590059,0.0066126458946318,
0.00664163284336301,0.00669960674082544,0.00675758063828786,0.00681555453575028,
0.00687352843321271,0.00693150233067513,0.00698947622813756,0.00701846317686877,
0.00704745012559998,0.00716339792052483,0.00727934571544968,0.0073373196129121,
0.00739529351037453,0.00742428045910574,0.00745326740783695,0.00751124130529938,
0.0075692152027618,0.00762718910022423,0.00768516299768665,0.00774313689514908,
0.0078011107926115,0.00783009774134271,0.00785908469007393),
 .UNSPECIFIED.);
#159=SHAPE_REPRESENTATION_RELATIONSHIP('SRR','None',#10586,#168);
#160=SHAPE_REPRESENTATION_RELATIONSHIP('SRR','None',#10587,#169);
#161=SHAPE_REPRESENTATION_RELATIONSHIP('SRR','None',#10588,#170);
#162=SHAPE_REPRESENTATION_RELATIONSHIP('SRR','None',#10589,#171);
#163=SHAPE_REPRESENTATION_RELATIONSHIP('SRR','None',#10590,#172);
#164=SHAPE_REPRESENTATION_RELATIONSHIP('SRR','None',#10591,#173);
#165=SHAPE_REPRESENTATION_RELATIONSHIP('SRR','None',#10592,#174);
#166=SHAPE_REPRESENTATION_RELATIONSHIP('SRR','None',#10593,#175);
#167=SHAPE_REPRESENTATION_RELATIONSHIP('SRR','None',#10594,#176);
#168=ADVANCED_BREP_SHAPE_REPRESENTATION('',(#187),#10542);
#169=ADVANCED_BREP_SHAPE_REPRESENTATION('',(#188),#10543);
#170=ADVANCED_BREP_SHAPE_REPRESENTATION('',(#189),#10544);
#171=ADVANCED_BREP_SHAPE_REPRESENTATION('',(#190),#10545);
#172=ADVANCED_BREP_SHAPE_REPRESENTATION('',(#191),#10546);
#173=ADVANCED_BREP_SHAPE_REPRESENTATION('',(#192),#10547);
#174=ADVANCED_BREP_SHAPE_REPRESENTATION('',(#193),#10548);
#175=ADVANCED_BREP_SHAPE_REPRESENTATION('',(#194),#10549);
#176=ADVANCED_BREP_SHAPE_REPRESENTATION('',(#195,#196),#10550);
#177=STYLED_ITEM('',(#10640),#187);
#178=STYLED_ITEM('',(#10641),#188);
#179=STYLED_ITEM('',(#10642),#189);
#180=STYLED_ITEM('',(#10640),#190);
#181=STYLED_ITEM('',(#10643),#191);
#182=STYLED_ITEM('',(#10644),#192);
#183=STYLED_ITEM('',(#10644),#193);
#184=STYLED_ITEM('',(#10644),#194);
#185=STYLED_ITEM('',(#10645),#195);
#186=STYLED_ITEM('',(#10645),#196);
#187=MANIFOLD_SOLID_BREP('Body1',#3426);
#188=MANIFOLD_SOLID_BREP('Body1',#3427);
#189=MANIFOLD_SOLID_BREP('Body1',#3428);
#190=MANIFOLD_SOLID_BREP('Body1',#3429);
#191=MANIFOLD_SOLID_BREP('Body1',#3430);
#192=MANIFOLD_SOLID_BREP('Body1',#3431);
#193=MANIFOLD_SOLID_BREP('Body1',#3432);
#194=MANIFOLD_SOLID_BREP('Body1',#3433);
#195=MANIFOLD_SOLID_BREP('Body1',#3434);
#196=MANIFOLD_SOLID_BREP('Body2',#3435);
#197=FACE_BOUND('',#522,.T.);
#198=FACE_BOUND('',#523,.T.);
#199=FACE_BOUND('',#525,.T.);
#200=FACE_BOUND('',#531,.T.);
#201=FACE_BOUND('',#533,.T.);
#202=FACE_BOUND('',#534,.T.);
#203=FACE_BOUND('',#549,.T.);
#204=FACE_BOUND('',#555,.T.);
#205=FACE_BOUND('',#557,.T.);
#206=FACE_BOUND('',#563,.T.);
#207=FACE_BOUND('',#565,.T.);
#208=FACE_BOUND('',#577,.T.);
#209=FACE_BOUND('',#579,.T.);
#210=FACE_BOUND('',#586,.T.);
#211=FACE_BOUND('',#588,.T.);
#212=FACE_BOUND('',#600,.T.);
#213=FACE_BOUND('',#601,.T.);
#214=FACE_BOUND('',#611,.T.);
#215=FACE_BOUND('',#613,.T.);
#216=FACE_BOUND('',#615,.T.);
#217=FACE_BOUND('',#618,.T.);
#218=FACE_BOUND('',#620,.T.);
#219=FACE_BOUND('',#625,.T.);
#220=FACE_BOUND('',#628,.T.);
#221=FACE_BOUND('',#658,.T.);
#222=FACE_BOUND('',#660,.T.);
#223=FACE_BOUND('',#757,.T.);
#224=PLANE('',#3547);
#225=PLANE('',#3548);
#226=PLANE('',#3549);
#227=PLANE('',#3550);
#228=PLANE('',#3551);
#229=PLANE('',#3552);
#230=PLANE('',#3553);
#231=PLANE('',#3554);
#232=PLANE('',#3559);
#233=PLANE('',#3564);
#234=PLANE('',#3565);
#235=PLANE('',#3566);
#236=PLANE('',#3571);
#237=PLANE('',#3572);
#238=PLANE('',#3573);
#239=PLANE('',#3574);
#240=PLANE('',#3575);
#241=PLANE('',#3576);
#242=PLANE('',#3587);
#243=PLANE('',#3588);
#244=PLANE('',#3589);
#245=PLANE('',#3590);
#246=PLANE('',#3591);
#247=PLANE('',#3592);
#248=PLANE('',#3597);
#249=PLANE('',#3602);
#250=PLANE('',#3603);
#251=PLANE('',#3604);
#252=PLANE('',#3605);
#253=PLANE('',#3606);
#254=PLANE('',#3611);
#255=PLANE('',#3631);
#256=PLANE('',#3632);
#257=PLANE('',#3637);
#258=PLANE('',#3638);
#259=PLANE('',#3639);
#260=PLANE('',#3640);
#261=PLANE('',#3641);
#262=PLANE('',#3642);
#263=PLANE('',#3643);
#264=PLANE('',#3644);
#265=PLANE('',#3645);
#266=PLANE('',#3646);
#267=PLANE('',#3647);
#268=PLANE('',#3648);
#269=PLANE('',#3649);
#270=PLANE('',#3650);
#271=PLANE('',#3680);
#272=PLANE('',#3681);
#273=PLANE('',#3682);
#274=PLANE('',#3683);
#275=PLANE('',#3684);
#276=PLANE('',#3685);
#277=PLANE('',#3686);
#278=PLANE('',#3687);
#279=PLANE('',#3688);
#280=PLANE('',#3689);
#281=PLANE('',#3690);
#282=PLANE('',#3701);
#283=PLANE('',#3707);
#284=PLANE('',#3758);
#285=PLANE('',#3763);
#286=PLANE('',#3768);
#287=PLANE('',#3773);
#288=PLANE('',#3778);
#289=PLANE('',#3783);
#290=PLANE('',#3788);
#291=PLANE('',#3794);
#292=PLANE('',#4011);
#293=PLANE('',#4026);
#294=FACE_OUTER_BOUND('',#514,.T.);
#295=FACE_OUTER_BOUND('',#515,.T.);
#296=FACE_OUTER_BOUND('',#516,.T.);
#297=FACE_OUTER_BOUND('',#517,.T.);
#298=FACE_OUTER_BOUND('',#518,.T.);
#299=FACE_OUTER_BOUND('',#519,.T.);
#300=FACE_OUTER_BOUND('',#520,.T.);
#301=FACE_OUTER_BOUND('',#521,.T.);
#302=FACE_OUTER_BOUND('',#524,.T.);
#303=FACE_OUTER_BOUND('',#526,.T.);
#304=FACE_OUTER_BOUND('',#527,.T.);
#305=FACE_OUTER_BOUND('',#528,.T.);
#306=FACE_OUTER_BOUND('',#529,.T.);
#307=FACE_OUTER_BOUND('',#530,.T.);
#308=FACE_OUTER_BOUND('',#532,.T.);
#309=FACE_OUTER_BOUND('',#535,.T.);
#310=FACE_OUTER_BOUND('',#536,.T.);
#311=FACE_OUTER_BOUND('',#537,.T.);
#312=FACE_OUTER_BOUND('',#538,.T.);
#313=FACE_OUTER_BOUND('',#539,.T.);
#314=FACE_OUTER_BOUND('',#540,.T.);
#315=FACE_OUTER_BOUND('',#541,.T.);
#316=FACE_OUTER_BOUND('',#542,.T.);
#317=FACE_OUTER_BOUND('',#543,.T.);
#318=FACE_OUTER_BOUND('',#544,.T.);
#319=FACE_OUTER_BOUND('',#545,.T.);
#320=FACE_OUTER_BOUND('',#546,.T.);
#321=FACE_OUTER_BOUND('',#547,.T.);
#322=FACE_OUTER_BOUND('',#548,.T.);
#323=FACE_OUTER_BOUND('',#550,.T.);
#324=FACE_OUTER_BOUND('',#551,.T.);
#325=FACE_OUTER_BOUND('',#552,.T.);
#326=FACE_OUTER_BOUND('',#553,.T.);
#327=FACE_OUTER_BOUND('',#554,.T.);
#328=FACE_OUTER_BOUND('',#556,.T.);
#329=FACE_OUTER_BOUND('',#558,.T.);
#330=FACE_OUTER_BOUND('',#559,.T.);
#331=FACE_OUTER_BOUND('',#560,.T.);
#332=FACE_OUTER_BOUND('',#561,.T.);
#333=FACE_OUTER_BOUND('',#562,.T.);
#334=FACE_OUTER_BOUND('',#564,.T.);
#335=FACE_OUTER_BOUND('',#566,.T.);
#336=FACE_OUTER_BOUND('',#567,.T.);
#337=FACE_OUTER_BOUND('',#568,.T.);
#338=FACE_OUTER_BOUND('',#569,.T.);
#339=FACE_OUTER_BOUND('',#570,.T.);
#340=FACE_OUTER_BOUND('',#571,.T.);
#341=FACE_OUTER_BOUND('',#572,.T.);
#342=FACE_OUTER_BOUND('',#573,.T.);
#343=FACE_OUTER_BOUND('',#574,.T.);
#344=FACE_OUTER_BOUND('',#575,.T.);
#345=FACE_OUTER_BOUND('',#576,.T.);
#346=FACE_OUTER_BOUND('',#578,.T.);
#347=FACE_OUTER_BOUND('',#580,.T.);
#348=FACE_OUTER_BOUND('',#581,.T.);
#349=FACE_OUTER_BOUND('',#582,.T.);
#350=FACE_OUTER_BOUND('',#583,.T.);
#351=FACE_OUTER_BOUND('',#584,.T.);
#352=FACE_OUTER_BOUND('',#585,.T.);
#353=FACE_OUTER_BOUND('',#587,.T.);
#354=FACE_OUTER_BOUND('',#589,.T.);
#355=FACE_OUTER_BOUND('',#590,.T.);
#356=FACE_OUTER_BOUND('',#591,.T.);
#357=FACE_OUTER_BOUND('',#592,.T.);
#358=FACE_OUTER_BOUND('',#593,.T.);
#359=FACE_OUTER_BOUND('',#594,.T.);
#360=FACE_OUTER_BOUND('',#595,.T.);
#361=FACE_OUTER_BOUND('',#596,.T.);
#362=FACE_OUTER_BOUND('',#597,.T.);
#363=FACE_OUTER_BOUND('',#598,.T.);
#364=FACE_OUTER_BOUND('',#599,.T.);
#365=FACE_OUTER_BOUND('',#602,.T.);
#366=FACE_OUTER_BOUND('',#603,.T.);
#367=FACE_OUTER_BOUND('',#604,.T.);
#368=FACE_OUTER_BOUND('',#605,.T.);
#369=FACE_OUTER_BOUND('',#606,.T.);
#370=FACE_OUTER_BOUND('',#607,.T.);
#371=FACE_OUTER_BOUND('',#608,.T.);
#372=FACE_OUTER_BOUND('',#609,.T.);
#373=FACE_OUTER_BOUND('',#610,.T.);
#374=FACE_OUTER_BOUND('',#612,.T.);
#375=FACE_OUTER_BOUND('',#614,.T.);
#376=FACE_OUTER_BOUND('',#616,.T.);
#377=FACE_OUTER_BOUND('',#617,.T.);
#378=FACE_OUTER_BOUND('',#619,.T.);
#379=FACE_OUTER_BOUND('',#621,.T.);
#380=FACE_OUTER_BOUND('',#622,.T.);
#381=FACE_OUTER_BOUND('',#623,.T.);
#382=FACE_OUTER_BOUND('',#624,.T.);
#383=FACE_OUTER_BOUND('',#626,.T.);
#384=FACE_OUTER_BOUND('',#627,.T.);
#385=FACE_OUTER_BOUND('',#629,.T.);
#386=FACE_OUTER_BOUND('',#630,.T.);
#387=FACE_OUTER_BOUND('',#631,.T.);
#388=FACE_OUTER_BOUND('',#632,.T.);
#389=FACE_OUTER_BOUND('',#633,.T.);
#390=FACE_OUTER_BOUND('',#634,.T.);
#391=FACE_OUTER_BOUND('',#635,.T.);
#392=FACE_OUTER_BOUND('',#636,.T.);
#393=FACE_OUTER_BOUND('',#637,.T.);
#394=FACE_OUTER_BOUND('',#638,.T.);
#395=FACE_OUTER_BOUND('',#639,.T.);
#396=FACE_OUTER_BOUND('',#640,.T.);
#397=FACE_OUTER_BOUND('',#641,.T.);
#398=FACE_OUTER_BOUND('',#642,.T.);
#399=FACE_OUTER_BOUND('',#643,.T.);
#400=FACE_OUTER_BOUND('',#644,.T.);
#401=FACE_OUTER_BOUND('',#645,.T.);
#402=FACE_OUTER_BOUND('',#646,.T.);
#403=FACE_OUTER_BOUND('',#647,.T.);
#404=FACE_OUTER_BOUND('',#648,.T.);
#405=FACE_OUTER_BOUND('',#649,.T.);
#406=FACE_OUTER_BOUND('',#650,.T.);
#407=FACE_OUTER_BOUND('',#651,.T.);
#408=FACE_OUTER_BOUND('',#652,.T.);
#409=FACE_OUTER_BOUND('',#653,.T.);
#410=FACE_OUTER_BOUND('',#654,.T.);
#411=FACE_OUTER_BOUND('',#655,.T.);
#412=FACE_OUTER_BOUND('',#656,.T.);
#413=FACE_OUTER_BOUND('',#657,.T.);
#414=FACE_OUTER_BOUND('',#659,.T.);
#415=FACE_OUTER_BOUND('',#661,.T.);
#416=FACE_OUTER_BOUND('',#662,.T.);
#417=FACE_OUTER_BOUND('',#663,.T.);
#418=FACE_OUTER_BOUND('',#664,.T.);
#419=FACE_OUTER_BOUND('',#665,.T.);
#420=FACE_OUTER_BOUND('',#666,.T.);
#421=FACE_OUTER_BOUND('',#667,.T.);
#422=FACE_OUTER_BOUND('',#668,.T.);
#423=FACE_OUTER_BOUND('',#669,.T.);
#424=FACE_OUTER_BOUND('',#670,.T.);
#425=FACE_OUTER_BOUND('',#671,.T.);
#426=FACE_OUTER_BOUND('',#672,.T.);
#427=FACE_OUTER_BOUND('',#673,.T.);
#428=FACE_OUTER_BOUND('',#674,.T.);
#429=FACE_OUTER_BOUND('',#675,.T.);
#430=FACE_OUTER_BOUND('',#676,.T.);
#431=FACE_OUTER_BOUND('',#677,.T.);
#432=FACE_OUTER_BOUND('',#678,.T.);
#433=FACE_OUTER_BOUND('',#679,.T.);
#434=FACE_OUTER_BOUND('',#680,.T.);
#435=FACE_OUTER_BOUND('',#681,.T.);
#436=FACE_OUTER_BOUND('',#682,.T.);
#437=FACE_OUTER_BOUND('',#683,.T.);
#438=FACE_OUTER_BOUND('',#684,.T.);
#439=FACE_OUTER_BOUND('',#685,.T.);
#440=FACE_OUTER_BOUND('',#686,.T.);
#441=FACE_OUTER_BOUND('',#687,.T.);
#442=FACE_OUTER_BOUND('',#688,.T.);
#443=FACE_OUTER_BOUND('',#689,.T.);
#444=FACE_OUTER_BOUND('',#690,.T.);
#445=FACE_OUTER_BOUND('',#691,.T.);
#446=FACE_OUTER_BOUND('',#692,.T.);
#447=FACE_OUTER_BOUND('',#693,.T.);
#448=FACE_OUTER_BOUND('',#694,.T.);
#449=FACE_OUTER_BOUND('',#695,.T.);
#450=FACE_OUTER_BOUND('',#696,.T.);
#451=FACE_OUTER_BOUND('',#697,.T.);
#452=FACE_OUTER_BOUND('',#698,.T.);
#453=FACE_OUTER_BOUND('',#699,.T.);
#454=FACE_OUTER_BOUND('',#700,.T.);
#455=FACE_OUTER_BOUND('',#701,.T.);
#456=FACE_OUTER_BOUND('',#702,.T.);
#457=FACE_OUTER_BOUND('',#703,.T.);
#458=FACE_OUTER_BOUND('',#704,.T.);
#459=FACE_OUTER_BOUND('',#705,.T.);
#460=FACE_OUTER_BOUND('',#706,.T.);
#461=FACE_OUTER_BOUND('',#707,.T.);
#462=FACE_OUTER_BOUND('',#708,.T.);
#463=FACE_OUTER_BOUND('',#709,.T.);
#464=FACE_OUTER_BOUND('',#710,.T.);
#465=FACE_OUTER_BOUND('',#711,.T.);
#466=FACE_OUTER_BOUND('',#712,.T.);
#467=FACE_OUTER_BOUND('',#713,.T.);
#468=FACE_OUTER_BOUND('',#714,.T.);
#469=FACE_OUTER_BOUND('',#715,.T.);
#470=FACE_OUTER_BOUND('',#716,.T.);
#471=FACE_OUTER_BOUND('',#717,.T.);
#472=FACE_OUTER_BOUND('',#718,.T.);
#473=FACE_OUTER_BOUND('',#719,.T.);
#474=FACE_OUTER_BOUND('',#720,.T.);
#475=FACE_OUTER_BOUND('',#721,.T.);
#476=FACE_OUTER_BOUND('',#722,.T.);
#477=FACE_OUTER_BOUND('',#723,.T.);
#478=FACE_OUTER_BOUND('',#724,.T.);
#479=FACE_OUTER_BOUND('',#725,.T.);
#480=FACE_OUTER_BOUND('',#726,.T.);
#481=FACE_OUTER_BOUND('',#727,.T.);
#482=FACE_OUTER_BOUND('',#728,.T.);
#483=FACE_OUTER_BOUND('',#729,.T.);
#484=FACE_OUTER_BOUND('',#730,.T.);
#485=FACE_OUTER_BOUND('',#731,.T.);
#486=FACE_OUTER_BOUND('',#732,.T.);
#487=FACE_OUTER_BOUND('',#733,.T.);
#488=FACE_OUTER_BOUND('',#734,.T.);
#489=FACE_OUTER_BOUND('',#735,.T.);
#490=FACE_OUTER_BOUND('',#736,.T.);
#491=FACE_OUTER_BOUND('',#737,.T.);
#492=FACE_OUTER_BOUND('',#738,.T.);
#493=FACE_OUTER_BOUND('',#739,.T.);
#494=FACE_OUTER_BOUND('',#740,.T.);
#495=FACE_OUTER_BOUND('',#741,.T.);
#496=FACE_OUTER_BOUND('',#742,.T.);
#497=FACE_OUTER_BOUND('',#743,.T.);
#498=FACE_OUTER_BOUND('',#744,.T.);
#499=FACE_OUTER_BOUND('',#745,.T.);
#500=FACE_OUTER_BOUND('',#746,.T.);
#501=FACE_OUTER_BOUND('',#747,.T.);
#502=FACE_OUTER_BOUND('',#748,.T.);
#503=FACE_OUTER_BOUND('',#749,.T.);
#504=FACE_OUTER_BOUND('',#750,.T.);
#505=FACE_OUTER_BOUND('',#751,.T.);
#506=FACE_OUTER_BOUND('',#752,.T.);
#507=FACE_OUTER_BOUND('',#753,.T.);
#508=FACE_OUTER_BOUND('',#754,.T.);
#509=FACE_OUTER_BOUND('',#755,.T.);
#510=FACE_OUTER_BOUND('',#756,.T.);
#511=FACE_OUTER_BOUND('',#758,.T.);
#512=FACE_OUTER_BOUND('',#759,.T.);
#513=FACE_OUTER_BOUND('',#760,.T.);
#514=EDGE_LOOP('',(#2188,#2189,#2190,#2191));
#515=EDGE_LOOP('',(#2192,#2193,#2194,#2195));
#516=EDGE_LOOP('',(#2196,#2197,#2198,#2199));
#517=EDGE_LOOP('',(#2200,#2201,#2202,#2203));
#518=EDGE_LOOP('',(#2204,#2205,#2206,#2207));
#519=EDGE_LOOP('',(#2208,#2209,#2210,#2211));
#520=EDGE_LOOP('',(#2212,#2213,#2214,#2215));
#521=EDGE_LOOP('',(#2216,#2217,#2218,#2219,#2220,#2221,#2222,#2223));
#522=EDGE_LOOP('',(#2224));
#523=EDGE_LOOP('',(#2225));
#524=EDGE_LOOP('',(#2226,#2227,#2228,#2229));
#525=EDGE_LOOP('',(#2230));
#526=EDGE_LOOP('',(#2231,#2232,#2233,#2234,#2235,#2236,#2237,#2238));
#527=EDGE_LOOP('',(#2239,#2240,#2241,#2242,#2243,#2244,#2245,#2246,#2247,
#2248,#2249,#2250));
#528=EDGE_LOOP('',(#2251,#2252,#2253,#2254,#2255,#2256,#2257,#2258,#2259,
#2260,#2261,#2262));
#529=EDGE_LOOP('',(#2263,#2264,#2265,#2266,#2267,#2268,#2269,#2270));
#530=EDGE_LOOP('',(#2271,#2272,#2273,#2274));
#531=EDGE_LOOP('',(#2275));
#532=EDGE_LOOP('',(#2276,#2277,#2278,#2279,#2280,#2281,#2282,#2283));
#533=EDGE_LOOP('',(#2284));
#534=EDGE_LOOP('',(#2285));
#535=EDGE_LOOP('',(#2286,#2287,#2288,#2289));
#536=EDGE_LOOP('',(#2290,#2291,#2292,#2293));
#537=EDGE_LOOP('',(#2294,#2295,#2296,#2297));
#538=EDGE_LOOP('',(#2298,#2299,#2300,#2301));
#539=EDGE_LOOP('',(#2302,#2303,#2304,#2305));
#540=EDGE_LOOP('',(#2306,#2307,#2308,#2309));
#541=EDGE_LOOP('',(#2310,#2311,#2312,#2313));
#542=EDGE_LOOP('',(#2314,#2315,#2316,#2317));
#543=EDGE_LOOP('',(#2318,#2319,#2320,#2321));
#544=EDGE_LOOP('',(#2322,#2323,#2324,#2325));
#545=EDGE_LOOP('',(#2326,#2327,#2328,#2329));
#546=EDGE_LOOP('',(#2330,#2331,#2332,#2333));
#547=EDGE_LOOP('',(#2334,#2335,#2336,#2337));
#548=EDGE_LOOP('',(#2338));
#549=EDGE_LOOP('',(#2339));
#550=EDGE_LOOP('',(#2340,#2341,#2342,#2343));
#551=EDGE_LOOP('',(#2344,#2345,#2346,#2347));
#552=EDGE_LOOP('',(#2348,#2349,#2350,#2351));
#553=EDGE_LOOP('',(#2352,#2353,#2354,#2355));
#554=EDGE_LOOP('',(#2356,#2357,#2358,#2359,#2360,#2361,#2362,#2363));
#555=EDGE_LOOP('',(#2364));
#556=EDGE_LOOP('',(#2365,#2366,#2367,#2368,#2369,#2370,#2371,#2372));
#557=EDGE_LOOP('',(#2373));
#558=EDGE_LOOP('',(#2374,#2375,#2376,#2377));
#559=EDGE_LOOP('',(#2378,#2379,#2380,#2381));
#560=EDGE_LOOP('',(#2382,#2383,#2384,#2385));
#561=EDGE_LOOP('',(#2386,#2387,#2388,#2389));
#562=EDGE_LOOP('',(#2390,#2391,#2392,#2393,#2394,#2395,#2396,#2397));
#563=EDGE_LOOP('',(#2398));
#564=EDGE_LOOP('',(#2399,#2400,#2401,#2402,#2403,#2404,#2405,#2406));
#565=EDGE_LOOP('',(#2407));
#566=EDGE_LOOP('',(#2408,#2409,#2410,#2411));
#567=EDGE_LOOP('',(#2412,#2413,#2414,#2415));
#568=EDGE_LOOP('',(#2416,#2417,#2418,#2419));
#569=EDGE_LOOP('',(#2420,#2421,#2422,#2423));
#570=EDGE_LOOP('',(#2424,#2425,#2426,#2427));
#571=EDGE_LOOP('',(#2428,#2429,#2430,#2431));
#572=EDGE_LOOP('',(#2432,#2433,#2434,#2435));
#573=EDGE_LOOP('',(#2436,#2437,#2438,#2439));
#574=EDGE_LOOP('',(#2440,#2441,#2442,#2443));
#575=EDGE_LOOP('',(#2444,#2445,#2446,#2447));
#576=EDGE_LOOP('',(#2448));
#577=EDGE_LOOP('',(#2449));
#578=EDGE_LOOP('',(#2450));
#579=EDGE_LOOP('',(#2451));
#580=EDGE_LOOP('',(#2452,#2453,#2454,#2455));
#581=EDGE_LOOP('',(#2456,#2457,#2458,#2459));
#582=EDGE_LOOP('',(#2460,#2461,#2462,#2463));
#583=EDGE_LOOP('',(#2464,#2465,#2466,#2467));
#584=EDGE_LOOP('',(#2468,#2469,#2470,#2471));
#585=EDGE_LOOP('',(#2472,#2473,#2474,#2475,#2476,#2477,#2478,#2479,#2480,
#2481,#2482,#2483));
#586=EDGE_LOOP('',(#2484));
#587=EDGE_LOOP('',(#2485,#2486,#2487,#2488,#2489,#2490,#2491,#2492,#2493,
#2494,#2495,#2496));
#588=EDGE_LOOP('',(#2497));
#589=EDGE_LOOP('',(#2498,#2499,#2500,#2501));
#590=EDGE_LOOP('',(#2502,#2503,#2504,#2505));
#591=EDGE_LOOP('',(#2506,#2507,#2508,#2509));
#592=EDGE_LOOP('',(#2510,#2511,#2512,#2513));
#593=EDGE_LOOP('',(#2514,#2515,#2516,#2517));
#594=EDGE_LOOP('',(#2518,#2519,#2520,#2521));
#595=EDGE_LOOP('',(#2522,#2523,#2524,#2525));
#596=EDGE_LOOP('',(#2526,#2527,#2528,#2529));
#597=EDGE_LOOP('',(#2530,#2531,#2532,#2533,#2534));
#598=EDGE_LOOP('',(#2535,#2536,#2537,#2538,#2539));
#599=EDGE_LOOP('',(#2540,#2541,#2542,#2543,#2544,#2545,#2546,#2547,#2548,
#2549,#2550,#2551));
#600=EDGE_LOOP('',(#2552,#2553));
#601=EDGE_LOOP('',(#2554,#2555));
#602=EDGE_LOOP('',(#2556,#2557,#2558,#2559,#2560,#2561));
#603=EDGE_LOOP('',(#2562,#2563,#2564,#2565,#2566,#2567));
#604=EDGE_LOOP('',(#2568,#2569,#2570,#2571));
#605=EDGE_LOOP('',(#2572,#2573,#2574,#2575));
#606=EDGE_LOOP('',(#2576,#2577,#2578,#2579));
#607=EDGE_LOOP('',(#2580,#2581,#2582,#2583));
#608=EDGE_LOOP('',(#2584,#2585,#2586,#2587));
#609=EDGE_LOOP('',(#2588,#2589,#2590,#2591));
#610=EDGE_LOOP('',(#2592));
#611=EDGE_LOOP('',(#2593));
#612=EDGE_LOOP('',(#2594));
#613=EDGE_LOOP('',(#2595));
#614=EDGE_LOOP('',(#2596));
#615=EDGE_LOOP('',(#2597));
#616=EDGE_LOOP('',(#2598));
#617=EDGE_LOOP('',(#2599));
#618=EDGE_LOOP('',(#2600));
#619=EDGE_LOOP('',(#2601));
#620=EDGE_LOOP('',(#2602));
#621=EDGE_LOOP('',(#2603,#2604,#2605,#2606));
#622=EDGE_LOOP('',(#2607,#2608,#2609,#2610));
#623=EDGE_LOOP('',(#2611,#2612));
#624=EDGE_LOOP('',(#2613,#2614,#2615,#2616));
#625=EDGE_LOOP('',(#2617));
#626=EDGE_LOOP('',(#2618,#2619,#2620,#2621,#2622));
#627=EDGE_LOOP('',(#2623,#2624,#2625,#2626));
#628=EDGE_LOOP('',(#2627));
#629=EDGE_LOOP('',(#2628,#2629));
#630=EDGE_LOOP('',(#2630,#2631,#2632,#2633));
#631=EDGE_LOOP('',(#2634,#2635,#2636,#2637));
#632=EDGE_LOOP('',(#2638,#2639,#2640,#2641));
#633=EDGE_LOOP('',(#2642,#2643,#2644,#2645,#2646,#2647,#2648,#2649));
#634=EDGE_LOOP('',(#2650,#2651,#2652,#2653,#2654,#2655,#2656,#2657));
#635=EDGE_LOOP('',(#2658,#2659,#2660,#2661));
#636=EDGE_LOOP('',(#2662,#2663,#2664,#2665));
#637=EDGE_LOOP('',(#2666,#2667,#2668,#2669));
#638=EDGE_LOOP('',(#2670,#2671,#2672,#2673));
#639=EDGE_LOOP('',(#2674,#2675,#2676,#2677));
#640=EDGE_LOOP('',(#2678,#2679,#2680,#2681));
#641=EDGE_LOOP('',(#2682,#2683,#2684,#2685));
#642=EDGE_LOOP('',(#2686,#2687,#2688,#2689));
#643=EDGE_LOOP('',(#2690,#2691,#2692,#2693));
#644=EDGE_LOOP('',(#2694,#2695,#2696,#2697));
#645=EDGE_LOOP('',(#2698,#2699,#2700));
#646=EDGE_LOOP('',(#2701,#2702,#2703,#2704));
#647=EDGE_LOOP('',(#2705,#2706,#2707));
#648=EDGE_LOOP('',(#2708,#2709,#2710));
#649=EDGE_LOOP('',(#2711,#2712,#2713));
#650=EDGE_LOOP('',(#2714,#2715,#2716));
#651=EDGE_LOOP('',(#2717,#2718,#2719,#2720,#2721,#2722,#2723,#2724));
#652=EDGE_LOOP('',(#2725,#2726,#2727,#2728,#2729,#2730,#2731,#2732));
#653=EDGE_LOOP('',(#2733,#2734,#2735,#2736,#2737,#2738,#2739,#2740));
#654=EDGE_LOOP('',(#2741,#2742,#2743,#2744,#2745,#2746,#2747,#2748));
#655=EDGE_LOOP('',(#2749,#2750,#2751,#2752,#2753,#2754,#2755,#2756));
#656=EDGE_LOOP('',(#2757,#2758,#2759,#2760,#2761,#2762,#2763,#2764));
#657=EDGE_LOOP('',(#2765,#2766,#2767,#2768,#2769,#2770,#2771,#2772,#2773,
#2774,#2775,#2776));
#658=EDGE_LOOP('',(#2777));
#659=EDGE_LOOP('',(#2778,#2779,#2780,#2781,#2782,#2783,#2784,#2785,#2786,
#2787,#2788,#2789));
#660=EDGE_LOOP('',(#2790));
#661=EDGE_LOOP('',(#2791,#2792,#2793));
#662=EDGE_LOOP('',(#2794,#2795,#2796));
#663=EDGE_LOOP('',(#2797,#2798,#2799));
#664=EDGE_LOOP('',(#2800,#2801,#2802,#2803,#2804));
#665=EDGE_LOOP('',(#2805,#2806,#2807));
#666=EDGE_LOOP('',(#2808,#2809,#2810));
#667=EDGE_LOOP('',(#2811,#2812,#2813));
#668=EDGE_LOOP('',(#2814,#2815,#2816));
#669=EDGE_LOOP('',(#2817,#2818,#2819));
#670=EDGE_LOOP('',(#2820,#2821,#2822,#2823));
#671=EDGE_LOOP('',(#2824,#2825,#2826,#2827));
#672=EDGE_LOOP('',(#2828,#2829,#2830,#2831));
#673=EDGE_LOOP('',(#2832,#2833,#2834,#2835));
#674=EDGE_LOOP('',(#2836,#2837,#2838,#2839));
#675=EDGE_LOOP('',(#2840,#2841,#2842));
#676=EDGE_LOOP('',(#2843,#2844,#2845));
#677=EDGE_LOOP('',(#2846,#2847,#2848));
#678=EDGE_LOOP('',(#2849,#2850,#2851));
#679=EDGE_LOOP('',(#2852,#2853,#2854,#2855));
#680=EDGE_LOOP('',(#2856,#2857,#2858,#2859));
#681=EDGE_LOOP('',(#2860,#2861,#2862,#2863));
#682=EDGE_LOOP('',(#2864,#2865,#2866,#2867));
#683=EDGE_LOOP('',(#2868,#2869,#2870,#2871));
#684=EDGE_LOOP('',(#2872,#2873,#2874,#2875));
#685=EDGE_LOOP('',(#2876,#2877,#2878,#2879));
#686=EDGE_LOOP('',(#2880,#2881,#2882,#2883));
#687=EDGE_LOOP('',(#2884,#2885,#2886));
#688=EDGE_LOOP('',(#2887,#2888,#2889));
#689=EDGE_LOOP('',(#2890,#2891,#2892));
#690=EDGE_LOOP('',(#2893,#2894,#2895));
#691=EDGE_LOOP('',(#2896,#2897,#2898));
#692=EDGE_LOOP('',(#2899,#2900,#2901));
#693=EDGE_LOOP('',(#2902,#2903,#2904,#2905));
#694=EDGE_LOOP('',(#2906,#2907,#2908,#2909));
#695=EDGE_LOOP('',(#2910,#2911,#2912,#2913));
#696=EDGE_LOOP('',(#2914,#2915,#2916,#2917));
#697=EDGE_LOOP('',(#2918,#2919,#2920,#2921));
#698=EDGE_LOOP('',(#2922,#2923,#2924,#2925));
#699=EDGE_LOOP('',(#2926,#2927,#2928,#2929));
#700=EDGE_LOOP('',(#2930,#2931,#2932,#2933));
#701=EDGE_LOOP('',(#2934,#2935,#2936));
#702=EDGE_LOOP('',(#2937,#2938,#2939));
#703=EDGE_LOOP('',(#2940,#2941,#2942));
#704=EDGE_LOOP('',(#2943,#2944,#2945));
#705=EDGE_LOOP('',(#2946,#2947,#2948));
#706=EDGE_LOOP('',(#2949,#2950,#2951));
#707=EDGE_LOOP('',(#2952,#2953,#2954,#2955));
#708=EDGE_LOOP('',(#2956,#2957,#2958,#2959));
#709=EDGE_LOOP('',(#2960,#2961,#2962,#2963));
#710=EDGE_LOOP('',(#2964,#2965,#2966,#2967));
#711=EDGE_LOOP('',(#2968,#2969,#2970,#2971));
#712=EDGE_LOOP('',(#2972,#2973,#2974,#2975));
#713=EDGE_LOOP('',(#2976,#2977,#2978,#2979));
#714=EDGE_LOOP('',(#2980,#2981,#2982,#2983));
#715=EDGE_LOOP('',(#2984,#2985,#2986,#2987));
#716=EDGE_LOOP('',(#2988,#2989,#2990));
#717=EDGE_LOOP('',(#2991,#2992,#2993));
#718=EDGE_LOOP('',(#2994,#2995,#2996));
#719=EDGE_LOOP('',(#2997,#2998,#2999));
#720=EDGE_LOOP('',(#3000,#3001,#3002));
#721=EDGE_LOOP('',(#3003,#3004,#3005));
#722=EDGE_LOOP('',(#3006,#3007,#3008));
#723=EDGE_LOOP('',(#3009,#3010,#3011,#3012,#3013));
#724=EDGE_LOOP('',(#3014,#3015,#3016,#3017,#3018));
#725=EDGE_LOOP('',(#3019,#3020,#3021,#3022));
#726=EDGE_LOOP('',(#3023,#3024,#3025,#3026));
#727=EDGE_LOOP('',(#3027,#3028,#3029,#3030));
#728=EDGE_LOOP('',(#3031,#3032,#3033,#3034));
#729=EDGE_LOOP('',(#3035,#3036,#3037,#3038));
#730=EDGE_LOOP('',(#3039,#3040,#3041,#3042));
#731=EDGE_LOOP('',(#3043,#3044,#3045,#3046));
#732=EDGE_LOOP('',(#3047,#3048,#3049));
#733=EDGE_LOOP('',(#3050,#3051,#3052));
#734=EDGE_LOOP('',(#3053,#3054,#3055));
#735=EDGE_LOOP('',(#3056,#3057,#3058));
#736=EDGE_LOOP('',(#3059,#3060,#3061,#3062));
#737=EDGE_LOOP('',(#3063,#3064,#3065,#3066));
#738=EDGE_LOOP('',(#3067,#3068,#3069,#3070));
#739=EDGE_LOOP('',(#3071,#3072,#3073,#3074));
#740=EDGE_LOOP('',(#3075,#3076,#3077,#3078));
#741=EDGE_LOOP('',(#3079,#3080,#3081,#3082));
#742=EDGE_LOOP('',(#3083,#3084,#3085));
#743=EDGE_LOOP('',(#3086,#3087,#3088));
#744=EDGE_LOOP('',(#3089,#3090,#3091));
#745=EDGE_LOOP('',(#3092,#3093,#3094));
#746=EDGE_LOOP('',(#3095,#3096,#3097,#3098));
#747=EDGE_LOOP('',(#3099,#3100,#3101,#3102));
#748=EDGE_LOOP('',(#3103,#3104,#3105,#3106));
#749=EDGE_LOOP('',(#3107,#3108,#3109,#3110));
#750=EDGE_LOOP('',(#3111,#3112,#3113));
#751=EDGE_LOOP('',(#3114,#3115,#3116));
#752=EDGE_LOOP('',(#3117,#3118,#3119,#3120));
#753=EDGE_LOOP('',(#3121));
#754=EDGE_LOOP('',(#3122,#3123,#3124,#3125));
#755=EDGE_LOOP('',(#3126,#3127,#3128,#3129));
#756=EDGE_LOOP('',(#3130,#3131,#3132,#3133));
#757=EDGE_LOOP('',(#3134,#3135,#3136,#3137));
#758=EDGE_LOOP('',(#3138,#3139,#3140,#3141,#3142));
#759=EDGE_LOOP('',(#3143,#3144,#3145,#3146,#3147));
#760=EDGE_LOOP('',(#3148,#3149));
#761=LINE('',#5239,#958);
#762=LINE('',#5245,#959);
#763=LINE('',#5251,#960);
#764=LINE('',#5256,#961);
#765=LINE('',#5258,#962);
#766=LINE('',#5260,#963);
#767=LINE('',#5261,#964);
#768=LINE('',#5265,#965);
#769=LINE('',#5267,#966);
#770=LINE('',#5269,#967);
#771=LINE('',#5270,#968);
#772=LINE('',#5274,#969);
#773=LINE('',#5276,#970);
#774=LINE('',#5278,#971);
#775=LINE('',#5279,#972);
#776=LINE('',#5283,#973);
#777=LINE('',#5285,#974);
#778=LINE('',#5287,#975);
#779=LINE('',#5288,#976);
#780=LINE('',#5291,#977);
#781=LINE('',#5293,#978);
#782=LINE('',#5294,#979);
#783=LINE('',#5296,#980);
#784=LINE('',#5298,#981);
#785=LINE('',#5299,#982);
#786=LINE('',#5303,#983);
#787=LINE('',#5305,#984);
#788=LINE('',#5307,#985);
#789=LINE('',#5308,#986);
#790=LINE('',#5312,#987);
#791=LINE('',#5313,#988);
#792=LINE('',#5315,#989);
#793=LINE('',#5317,#990);
#794=LINE('',#5318,#991);
#795=LINE('',#5319,#992);
#796=LINE('',#5324,#993);
#797=LINE('',#5328,#994);
#798=LINE('',#5331,#995);
#799=LINE('',#5335,#996);
#800=LINE('',#5339,#997);
#801=LINE('',#5342,#998);
#802=LINE('',#5346,#999);
#803=LINE('',#5348,#1000);
#804=LINE('',#5349,#1001);
#805=LINE('',#5350,#1002);
#806=LINE('',#5352,#1003);
#807=LINE('',#5353,#1004);
#808=LINE('',#5357,#1005);
#809=LINE('',#5358,#1006);
#810=LINE('',#5359,#1007);
#811=LINE('',#5360,#1008);
#812=LINE('',#5366,#1009);
#813=LINE('',#5368,#1010);
#814=LINE('',#5371,#1011);
#815=LINE('',#5373,#1012);
#816=LINE('',#5380,#1013);
#817=LINE('',#5386,#1014);
#818=LINE('',#5392,#1015);
#819=LINE('',#5398,#1016);
#820=LINE('',#5400,#1017);
#821=LINE('',#5402,#1018);
#822=LINE('',#5403,#1019);
#823=LINE('',#5407,#1020);
#824=LINE('',#5409,#1021);
#825=LINE('',#5411,#1022);
#826=LINE('',#5412,#1023);
#827=LINE('',#5416,#1024);
#828=LINE('',#5418,#1025);
#829=LINE('',#5420,#1026);
#830=LINE('',#5421,#1027);
#831=LINE('',#5425,#1028);
#832=LINE('',#5427,#1029);
#833=LINE('',#5429,#1030);
#834=LINE('',#5430,#1031);
#835=LINE('',#5444,#1032);
#836=LINE('',#5446,#1033);
#837=LINE('',#5448,#1034);
#838=LINE('',#5449,#1035);
#839=LINE('',#5453,#1036);
#840=LINE('',#5455,#1037);
#841=LINE('',#5457,#1038);
#842=LINE('',#5458,#1039);
#843=LINE('',#5462,#1040);
#844=LINE('',#5464,#1041);
#845=LINE('',#5466,#1042);
#846=LINE('',#5467,#1043);
#847=LINE('',#5471,#1044);
#848=LINE('',#5473,#1045);
#849=LINE('',#5475,#1046);
#850=LINE('',#5476,#1047);
#851=LINE('',#5500,#1048);
#852=LINE('',#5506,#1049);
#853=LINE('',#5515,#1050);
#854=LINE('',#5520,#1051);
#855=LINE('',#5522,#1052);
#856=LINE('',#5524,#1053);
#857=LINE('',#5525,#1054);
#858=LINE('',#5529,#1055);
#859=LINE('',#5531,#1056);
#860=LINE('',#5533,#1057);
#861=LINE('',#5534,#1058);
#862=LINE('',#5538,#1059);
#863=LINE('',#5540,#1060);
#864=LINE('',#5542,#1061);
#865=LINE('',#5543,#1062);
#866=LINE('',#5547,#1063);
#867=LINE('',#5549,#1064);
#868=LINE('',#5551,#1065);
#869=LINE('',#5552,#1066);
#870=LINE('',#5555,#1067);
#871=LINE('',#5556,#1068);
#872=LINE('',#5558,#1069);
#873=LINE('',#5559,#1070);
#874=LINE('',#5561,#1071);
#875=LINE('',#5562,#1072);
#876=LINE('',#5564,#1073);
#877=LINE('',#5565,#1074);
#878=LINE('',#5568,#1075);
#879=LINE('',#5569,#1076);
#880=LINE('',#5571,#1077);
#881=LINE('',#5572,#1078);
#882=LINE('',#5574,#1079);
#883=LINE('',#5575,#1080);
#884=LINE('',#5577,#1081);
#885=LINE('',#5578,#1082);
#886=LINE('',#5580,#1083);
#887=LINE('',#5583,#1084);
#888=LINE('',#5586,#1085);
#889=LINE('',#5589,#1086);
#890=LINE('',#6109,#1087);
#891=LINE('',#6140,#1088);
#892=LINE('',#6658,#1089);
#893=LINE('',#6689,#1090);
#894=LINE('',#6695,#1091);
#895=LINE('',#6699,#1092);
#896=LINE('',#6703,#1093);
#897=LINE('',#6708,#1094);
#898=LINE('',#6711,#1095);
#899=LINE('',#6758,#1096);
#900=LINE('',#6785,#1097);
#901=LINE('',#6812,#1098);
#902=LINE('',#6818,#1099);
#903=LINE('',#6823,#1100);
#904=LINE('',#6828,#1101);
#905=LINE('',#6834,#1102);
#906=LINE('',#6840,#1103);
#907=LINE('',#7833,#1104);
#908=LINE('',#7835,#1105);
#909=LINE('',#7837,#1106);
#910=LINE('',#7839,#1107);
#911=LINE('',#7847,#1108);
#912=LINE('',#7850,#1109);
#913=LINE('',#7856,#1110);
#914=LINE('',#7859,#1111);
#915=LINE('',#7864,#1112);
#916=LINE('',#7885,#1113);
#917=LINE('',#7886,#1114);
#918=LINE('',#7889,#1115);
#919=LINE('',#7897,#1116);
#920=LINE('',#7902,#1117);
#921=LINE('',#7917,#1118);
#922=LINE('',#7920,#1119);
#923=LINE('',#7938,#1120);
#924=LINE('',#7970,#1121);
#925=LINE('',#7974,#1122);
#926=LINE('',#7978,#1123);
#927=LINE('',#7982,#1124);
#928=LINE('',#7989,#1125);
#929=LINE('',#7993,#1126);
#930=LINE('',#7997,#1127);
#931=LINE('',#8000,#1128);
#932=LINE('',#8006,#1129);
#933=LINE('',#8010,#1130);
#934=LINE('',#8014,#1131);
#935=LINE('',#8017,#1132);
#936=LINE('',#8023,#1133);
#937=LINE('',#8027,#1134);
#938=LINE('',#8031,#1135);
#939=LINE('',#8034,#1136);
#940=LINE('',#8039,#1137);
#941=LINE('',#8043,#1138);
#942=LINE('',#8047,#1139);
#943=LINE('',#8054,#1140);
#944=LINE('',#8059,#1141);
#945=LINE('',#8062,#1142);
#946=LINE('',#8068,#1143);
#947=LINE('',#8071,#1144);
#948=LINE('',#8073,#1145);
#949=LINE('',#8077,#1146);
#950=LINE('',#8081,#1147);
#951=LINE('',#8084,#1148);
#952=LINE('',#8088,#1149);
#953=LINE('',#8091,#1150);
#954=LINE('',#8093,#1151);
#955=LINE('',#8097,#1152);
#956=LINE('',#8101,#1153);
#957=LINE('',#8105,#1154);
#958=VECTOR('',#4044,1.225);
#959=VECTOR('',#4051,1.225);
#960=VECTOR('',#4058,1.65);
#961=VECTOR('',#4063,1000.);
#962=VECTOR('',#4064,1000.);
#963=VECTOR('',#4065,1000.);
#964=VECTOR('',#4066,1000.);
#965=VECTOR('',#4069,1000.);
#966=VECTOR('',#4070,1000.);
#967=VECTOR('',#4071,1000.);
#968=VECTOR('',#4072,1000.);
#969=VECTOR('',#4075,1000.);
#970=VECTOR('',#4076,1000.);
#971=VECTOR('',#4077,1000.);
#972=VECTOR('',#4078,1000.);
#973=VECTOR('',#4081,1000.);
#974=VECTOR('',#4082,1000.);
#975=VECTOR('',#4083,1000.);
#976=VECTOR('',#4084,1000.);
#977=VECTOR('',#4087,1000.);
#978=VECTOR('',#4088,1000.);
#979=VECTOR('',#4089,1000.);
#980=VECTOR('',#4090,1000.);
#981=VECTOR('',#4091,1000.);
#982=VECTOR('',#4092,1000.);
#983=VECTOR('',#4095,1000.);
#984=VECTOR('',#4096,1000.);
#985=VECTOR('',#4097,1000.);
#986=VECTOR('',#4098,1000.);
#987=VECTOR('',#4101,1000.);
#988=VECTOR('',#4102,1000.);
#989=VECTOR('',#4103,1000.);
#990=VECTOR('',#4104,1000.);
#991=VECTOR('',#4105,1000.);
#992=VECTOR('',#4106,1000.);
#993=VECTOR('',#4113,1000.);
#994=VECTOR('',#4116,1000.);
#995=VECTOR('',#4119,1000.);
#996=VECTOR('',#4124,1000.);
#997=VECTOR('',#4127,1000.);
#998=VECTOR('',#4130,1000.);
#999=VECTOR('',#4135,1000.);
#1000=VECTOR('',#4136,1000.);
#1001=VECTOR('',#4137,1000.);
#1002=VECTOR('',#4138,1000.);
#1003=VECTOR('',#4141,1000.);
#1004=VECTOR('',#4142,1000.);
#1005=VECTOR('',#4145,1000.);
#1006=VECTOR('',#4146,1000.);
#1007=VECTOR('',#4147,1000.);
#1008=VECTOR('',#4148,1000.);
#1009=VECTOR('',#4159,1000.);
#1010=VECTOR('',#4162,1000.);
#1011=VECTOR('',#4167,1000.);
#1012=VECTOR('',#4170,1000.);
#1013=VECTOR('',#4179,3.075);
#1014=VECTOR('',#4186,4.1);
#1015=VECTOR('',#4193,4.1);
#1016=VECTOR('',#4200,1000.);
#1017=VECTOR('',#4201,1000.);
#1018=VECTOR('',#4202,1000.);
#1019=VECTOR('',#4203,1000.);
#1020=VECTOR('',#4206,1000.);
#1021=VECTOR('',#4207,1000.);
#1022=VECTOR('',#4208,1000.);
#1023=VECTOR('',#4209,1000.);
#1024=VECTOR('',#4212,1000.);
#1025=VECTOR('',#4213,1000.);
#1026=VECTOR('',#4214,1000.);
#1027=VECTOR('',#4215,1000.);
#1028=VECTOR('',#4218,1000.);
#1029=VECTOR('',#4219,1000.);
#1030=VECTOR('',#4220,1000.);
#1031=VECTOR('',#4221,1000.);
#1032=VECTOR('',#4244,1000.);
#1033=VECTOR('',#4245,1000.);
#1034=VECTOR('',#4246,1000.);
#1035=VECTOR('',#4247,1000.);
#1036=VECTOR('',#4250,1000.);
#1037=VECTOR('',#4251,1000.);
#1038=VECTOR('',#4252,1000.);
#1039=VECTOR('',#4253,1000.);
#1040=VECTOR('',#4256,1000.);
#1041=VECTOR('',#4257,1000.);
#1042=VECTOR('',#4258,1000.);
#1043=VECTOR('',#4259,1000.);
#1044=VECTOR('',#4262,1000.);
#1045=VECTOR('',#4263,1000.);
#1046=VECTOR('',#4264,1000.);
#1047=VECTOR('',#4265,1000.);
#1048=VECTOR('',#4308,6.3);
#1049=VECTOR('',#4315,4.1);
#1050=VECTOR('',#4328,4.2);
#1051=VECTOR('',#4333,1000.);
#1052=VECTOR('',#4334,1000.);
#1053=VECTOR('',#4335,1000.);
#1054=VECTOR('',#4336,1000.);
#1055=VECTOR('',#4339,1000.);
#1056=VECTOR('',#4340,1000.);
#1057=VECTOR('',#4341,1000.);
#1058=VECTOR('',#4342,1000.);
#1059=VECTOR('',#4345,1000.);
#1060=VECTOR('',#4346,1000.);
#1061=VECTOR('',#4347,1000.);
#1062=VECTOR('',#4348,1000.);
#1063=VECTOR('',#4351,1000.);
#1064=VECTOR('',#4352,1000.);
#1065=VECTOR('',#4353,1000.);
#1066=VECTOR('',#4354,1000.);
#1067=VECTOR('',#4357,1000.);
#1068=VECTOR('',#4358,1000.);
#1069=VECTOR('',#4359,1000.);
#1070=VECTOR('',#4360,1000.);
#1071=VECTOR('',#4361,1000.);
#1072=VECTOR('',#4362,1000.);
#1073=VECTOR('',#4363,1000.);
#1074=VECTOR('',#4364,1000.);
#1075=VECTOR('',#4367,1000.);
#1076=VECTOR('',#4368,1000.);
#1077=VECTOR('',#4369,1000.);
#1078=VECTOR('',#4370,1000.);
#1079=VECTOR('',#4371,1000.);
#1080=VECTOR('',#4372,1000.);
#1081=VECTOR('',#4373,1000.);
#1082=VECTOR('',#4374,1000.);
#1083=VECTOR('',#4377,1000.);
#1084=VECTOR('',#4382,1000.);
#1085=VECTOR('',#4387,1000.);
#1086=VECTOR('',#4392,1000.);
#1087=VECTOR('',#4397,10.);
#1088=VECTOR('',#4398,10.);
#1089=VECTOR('',#4399,10.);
#1090=VECTOR('',#4400,10.);
#1091=VECTOR('',#4405,1000.);
#1092=VECTOR('',#4408,1000.);
#1093=VECTOR('',#4411,3.);
#1094=VECTOR('',#4416,1000.);
#1095=VECTOR('',#4419,1000.);
#1096=VECTOR('',#4422,1.);
#1097=VECTOR('',#4429,1.);
#1098=VECTOR('',#4434,2.3);
#1099=VECTOR('',#4441,1.14999999999999);
#1100=VECTOR('',#4448,1.14999999999999);
#1101=VECTOR('',#4453,1.49999999999999);
#1102=VECTOR('',#4460,1.99999999999999);
#1103=VECTOR('',#4467,3.);
#1104=VECTOR('',#4484,1000.);
#1105=VECTOR('',#4487,1000.);
#1106=VECTOR('',#4490,1000.);
#1107=VECTOR('',#4493,1000.);
#1108=VECTOR('',#4502,1000.);
#1109=VECTOR('',#4505,1000.);
#1110=VECTOR('',#4510,1000.);
#1111=VECTOR('',#4513,1000.);
#1112=VECTOR('',#4518,1000.);
#1113=VECTOR('',#4547,1000.);
#1114=VECTOR('',#4548,1000.);
#1115=VECTOR('',#4553,1000.);
#1116=VECTOR('',#4564,1.15);
#1117=VECTOR('',#4571,1.15);
#1118=VECTOR('',#4586,1000.);
#1119=VECTOR('',#4589,1000.);
#1120=VECTOR('',#4610,2.525);
#1121=VECTOR('',#4645,1000.);
#1122=VECTOR('',#4648,1000.);
#1123=VECTOR('',#4651,1000.);
#1124=VECTOR('',#4654,1000.);
#1125=VECTOR('',#4661,1000.);
#1126=VECTOR('',#4664,1000.);
#1127=VECTOR('',#4667,1000.);
#1128=VECTOR('',#4670,1000.);
#1129=VECTOR('',#4675,1000.);
#1130=VECTOR('',#4678,1000.);
#1131=VECTOR('',#4681,1000.);
#1132=VECTOR('',#4684,1000.);
#1133=VECTOR('',#4689,1000.);
#1134=VECTOR('',#4692,1000.);
#1135=VECTOR('',#4695,1000.);
#1136=VECTOR('',#4698,1000.);
#1137=VECTOR('',#4703,1000.);
#1138=VECTOR('',#4706,1000.);
#1139=VECTOR('',#4709,1000.);
#1140=VECTOR('',#4716,1000.);
#1141=VECTOR('',#4721,1000.);
#1142=VECTOR('',#4724,1000.);
#1143=VECTOR('',#4729,1000.);
#1144=VECTOR('',#4732,1000.);
#1145=VECTOR('',#4733,1000.);
#1146=VECTOR('',#4736,1000.);
#1147=VECTOR('',#4739,1000.);
#1148=VECTOR('',#4742,1000.);
#1149=VECTOR('',#4745,1000.);
#1150=VECTOR('',#4748,1000.);
#1151=VECTOR('',#4749,1000.);
#1152=VECTOR('',#4752,1000.);
#1153=VECTOR('',#4755,1000.);
#1154=VECTOR('',#4758,1000.);
#1155=CIRCLE('',#3539,1.225);
#1156=CIRCLE('',#3540,1.225);
#1157=CIRCLE('',#3542,1.225);
#1158=CIRCLE('',#3543,1.225);
#1159=CIRCLE('',#3545,1.65);
#1160=CIRCLE('',#3546,1.65);
#1161=CIRCLE('',#3555,1.);
#1162=CIRCLE('',#3556,1.);
#1163=CIRCLE('',#3557,0.2);
#1164=CIRCLE('',#3558,0.2);
#1165=CIRCLE('',#3560,1.);
#1166=CIRCLE('',#3561,0.2);
#1167=CIRCLE('',#3562,0.2);
#1168=CIRCLE('',#3563,1.);
#1169=CIRCLE('',#3579,3.075);
#1170=CIRCLE('',#3580,3.075);
#1171=CIRCLE('',#3582,4.1);
#1172=CIRCLE('',#3583,4.1);
#1173=CIRCLE('',#3585,4.1);
#1174=CIRCLE('',#3586,4.1);
#1175=CIRCLE('',#3593,0.5);
#1176=CIRCLE('',#3594,0.5);
#1177=CIRCLE('',#3595,0.5);
#1178=CIRCLE('',#3596,0.5);
#1179=CIRCLE('',#3598,0.5);
#1180=CIRCLE('',#3599,0.5);
#1181=CIRCLE('',#3600,0.5);
#1182=CIRCLE('',#3601,0.5);
#1183=CIRCLE('',#3607,0.5);
#1184=CIRCLE('',#3608,0.5);
#1185=CIRCLE('',#3609,0.5);
#1186=CIRCLE('',#3610,0.5);
#1187=CIRCLE('',#3612,0.5);
#1188=CIRCLE('',#3613,0.5);
#1189=CIRCLE('',#3614,0.5);
#1190=CIRCLE('',#3615,0.5);
#1191=CIRCLE('',#3626,6.3);
#1192=CIRCLE('',#3627,6.3);
#1193=CIRCLE('',#3629,4.1);
#1194=CIRCLE('',#3630,4.1);
#1195=CIRCLE('',#3635,4.2);
#1196=CIRCLE('',#3636,4.2);
#1197=CIRCLE('',#3653,3.);
#1198=CIRCLE('',#3654,3.);
#1199=CIRCLE('',#3655,3.);
#1200=CIRCLE('',#3656,3.);
#1201=CIRCLE('',#3657,3.);
#1202=CIRCLE('',#3658,3.);
#1203=CIRCLE('',#3660,1.);
#1204=CIRCLE('',#3662,1.);
#1205=CIRCLE('',#3664,2.3);
#1206=CIRCLE('',#3665,2.3);
#1207=CIRCLE('',#3667,1.14999999999999);
#1208=CIRCLE('',#3668,0.949999999999971);
#1209=CIRCLE('',#3670,1.14999999999999);
#1210=CIRCLE('',#3672,1.49999999999999);
#1211=CIRCLE('',#3673,1.49999999999999);
#1212=CIRCLE('',#3675,2.49999999999999);
#1213=CIRCLE('',#3676,1.99999999999999);
#1214=CIRCLE('',#3678,3.);
#1215=CIRCLE('',#3679,2.99999999999999);
#1216=CIRCLE('',#3693,1.1);
#1217=CIRCLE('',#3694,1.1);
#1218=CIRCLE('',#3696,1.7);
#1219=CIRCLE('',#3697,1.7);
#1220=CIRCLE('',#3699,5.);
#1221=CIRCLE('',#3700,5.);
#1222=CIRCLE('',#3702,6.);
#1223=CIRCLE('',#3703,1.1);
#1224=CIRCLE('',#3704,6.);
#1225=CIRCLE('',#3705,1.7);
#1226=CIRCLE('',#3706,1.5);
#1227=CIRCLE('',#3708,1.1);
#1228=CIRCLE('',#3709,6.);
#1229=CIRCLE('',#3710,1.5);
#1230=CIRCLE('',#3711,1.7);
#1231=CIRCLE('',#3712,6.);
#1232=CIRCLE('',#3720,1.15);
#1233=CIRCLE('',#3721,1.35);
#1234=CIRCLE('',#3723,1.15);
#1235=CIRCLE('',#3725,2.70416345659799);
#1236=CIRCLE('',#3726,0.05);
#1237=CIRCLE('',#3727,2.72688751925848);
#1238=CIRCLE('',#3728,0.0499999999999998);
#1239=CIRCLE('',#3730,0.05);
#1240=CIRCLE('',#3731,0.05);
#1241=CIRCLE('',#3733,2.72688751925848);
#1242=CIRCLE('',#3734,0.0500000000000001);
#1243=CIRCLE('',#3735,2.70416345659799);
#1244=CIRCLE('',#3736,0.0499999999999998);
#1245=CIRCLE('',#3738,2.525);
#1246=CIRCLE('',#3739,2.525);
#1247=CIRCLE('',#3741,2.525);
#1248=CIRCLE('',#3743,2.72688751925848);
#1249=CIRCLE('',#3744,5.37205536882039);
#1250=CIRCLE('',#3745,5.37205536882038);
#1251=CIRCLE('',#3747,2.72688751925848);
#1252=CIRCLE('',#3748,5.37205536882038);
#1253=CIRCLE('',#3749,5.37205536882038);
#1254=CIRCLE('',#3751,2.72688751925848);
#1255=CIRCLE('',#3752,5.37205536882039);
#1256=CIRCLE('',#3753,5.37205536882039);
#1257=CIRCLE('',#3755,2.72688751925848);
#1258=CIRCLE('',#3756,5.37205536882039);
#1259=CIRCLE('',#3757,5.37205536882038);
#1260=CIRCLE('',#3759,5.32728824074688);
#1261=CIRCLE('',#3760,5.32728824074688);
#1262=CIRCLE('',#3761,5.32728824074688);
#1263=CIRCLE('',#3762,5.32728824074688);
#1264=CIRCLE('',#3764,5.32728824074688);
#1265=CIRCLE('',#3765,5.32728824074688);
#1266=CIRCLE('',#3766,5.32728824074688);
#1267=CIRCLE('',#3767,5.32728824074688);
#1268=CIRCLE('',#3769,5.32728824074688);
#1269=CIRCLE('',#3770,5.32728824074688);
#1270=CIRCLE('',#3771,5.32728824074688);
#1271=CIRCLE('',#3772,5.32728824074688);
#1272=CIRCLE('',#3774,5.32728824074688);
#1273=CIRCLE('',#3775,5.32728824074688);
#1274=CIRCLE('',#3776,5.32728824074688);
#1275=CIRCLE('',#3777,5.32728824074688);
#1276=CIRCLE('',#3779,5.32728824074688);
#1277=CIRCLE('',#3780,5.32728824074688);
#1278=CIRCLE('',#3781,5.32728824074688);
#1279=CIRCLE('',#3782,5.32728824074688);
#1280=CIRCLE('',#3784,5.32728824074688);
#1281=CIRCLE('',#3785,5.32728824074688);
#1282=CIRCLE('',#3786,5.32728824074688);
#1283=CIRCLE('',#3787,5.32728824074688);
#1284=CIRCLE('',#3789,2.71615537110821);
#1285=CIRCLE('',#3790,2.70416345659799);
#1286=CIRCLE('',#3791,2.70416345659799);
#1287=CIRCLE('',#3792,2.70416345659799);
#1288=CIRCLE('',#3793,2.70416345659799);
#1289=CIRCLE('',#3795,2.70416345659799);
#1290=CIRCLE('',#3796,2.70416345659799);
#1291=CIRCLE('',#3797,2.70416345659799);
#1292=CIRCLE('',#3798,2.70416345659799);
#1293=CIRCLE('',#3799,2.70416345659799);
#1294=CIRCLE('',#3801,5.37205536882039);
#1295=CIRCLE('',#3802,5.37205536882038);
#1296=CIRCLE('',#3804,5.37205536882039);
#1297=CIRCLE('',#3805,5.37205536882038);
#1298=CIRCLE('',#3806,2.72688751925848);
#1299=CIRCLE('',#3808,5.37205536882038);
#1300=CIRCLE('',#3809,5.37205536882038);
#1301=CIRCLE('',#3810,2.72688751925848);
#1302=CIRCLE('',#3812,5.37205536882038);
#1303=CIRCLE('',#3813,5.37205536882039);
#1304=CIRCLE('',#3815,5.37205536882039);
#1305=CIRCLE('',#3816,5.37205536882038);
#1306=CIRCLE('',#3818,2.72688751925848);
#1307=CIRCLE('',#3819,5.37205536882038);
#1308=CIRCLE('',#3820,5.37205536882039);
#1309=CIRCLE('',#3822,2.72688751925848);
#1310=CIRCLE('',#3823,5.37205536882039);
#1311=CIRCLE('',#3824,5.37205536882038);
#1312=CIRCLE('',#3826,2.72688751925848);
#1313=CIRCLE('',#3827,5.37205536882039);
#1314=CIRCLE('',#3828,5.37205536882039);
#1315=CIRCLE('',#3830,0.0499999999999999);
#1316=CIRCLE('',#3831,0.0500000000000001);
#1317=CIRCLE('',#3832,0.05);
#1318=CIRCLE('',#3834,0.0500000000000001);
#1319=CIRCLE('',#3836,0.0500000000000001);
#1320=CIRCLE('',#3838,0.0499999999999998);
#1321=CIRCLE('',#3839,0.0500000000000002);
#1322=CIRCLE('',#3841,0.0499999999999999);
#1323=CIRCLE('',#3843,0.0500000000000002);
#1324=CIRCLE('',#3844,0.05);
#1325=CIRCLE('',#3846,0.0500000000000001);
#1326=CIRCLE('',#3848,0.0499999999999999);
#1327=CIRCLE('',#3850,0.0499999999999999);
#1328=CIRCLE('',#3852,0.0499999999999999);
#1329=CIRCLE('',#3853,0.05);
#1330=CIRCLE('',#3855,0.05);
#1331=CIRCLE('',#3857,0.0499999999999998);
#1332=CIRCLE('',#3859,0.0500000000000001);
#1333=CIRCLE('',#3861,0.0499999999999999);
#1334=CIRCLE('',#3863,0.05);
#1335=CIRCLE('',#3864,0.0500000000000001);
#1336=CIRCLE('',#3866,0.05);
#1337=CIRCLE('',#3867,0.0500000000000001);
#1338=CIRCLE('',#3869,0.05);
#1339=CIRCLE('',#3870,0.05);
#1340=CIRCLE('',#3872,0.0500000000000001);
#1341=CIRCLE('',#3874,0.0500000000000002);
#1342=CIRCLE('',#3876,0.0500000000000001);
#1343=CIRCLE('',#3878,0.05);
#1344=CIRCLE('',#3880,0.0499999999999999);
#1345=CIRCLE('',#3882,0.0499999999999999);
#1346=CIRCLE('',#3884,0.05);
#1347=CIRCLE('',#3886,0.05);
#1348=CIRCLE('',#3888,0.0500000000000001);
#1349=CIRCLE('',#3889,0.0500000000000001);
#1350=CIRCLE('',#3891,0.0500000000000001);
#1351=CIRCLE('',#3893,0.0500000000000002);
#1352=CIRCLE('',#3895,0.0499999999999999);
#1353=CIRCLE('',#3897,0.0500000000000001);
#1354=CIRCLE('',#3899,0.0500000000000001);
#1355=CIRCLE('',#3901,0.0500000000000001);
#1356=CIRCLE('',#3902,0.0499999999999999);
#1357=CIRCLE('',#3904,0.0500000000000001);
#1358=CIRCLE('',#3906,0.05);
#1359=CIRCLE('',#3908,0.05);
#1360=CIRCLE('',#3910,0.0500000000000002);
#1361=CIRCLE('',#3912,0.0500000000000002);
#1362=CIRCLE('',#3914,0.0499999999999999);
#1363=CIRCLE('',#3916,0.0500000000000001);
#1364=CIRCLE('',#3918,0.0500000000000001);
#1365=CIRCLE('',#3920,0.0499999999999999);
#1366=CIRCLE('',#3921,0.0500000000000001);
#1367=CIRCLE('',#3923,0.0500000000000002);
#1368=CIRCLE('',#3925,0.05);
#1369=CIRCLE('',#3927,0.0500000000000001);
#1370=CIRCLE('',#3928,0.0499999999999999);
#1371=CIRCLE('',#3930,0.0500000000000001);
#1372=CIRCLE('',#3932,0.0500000000000001);
#1373=CIRCLE('',#3934,0.0500000000000001);
#1374=CIRCLE('',#3935,0.0500000000000001);
#1375=CIRCLE('',#3937,0.0500000000000001);
#1376=CIRCLE('',#3939,0.0500000000000002);
#1377=CIRCLE('',#3940,0.0500000000000001);
#1378=CIRCLE('',#3942,0.05);
#1379=CIRCLE('',#3944,0.05);
#1380=CIRCLE('',#3947,0.05);
#1381=CIRCLE('',#3949,0.0500000000000001);
#1382=CIRCLE('',#3951,0.0500702725160199);
#1383=CIRCLE('',#3953,0.0500702740290074);
#1384=CIRCLE('',#3955,0.05);
#1385=CIRCLE('',#3957,0.05);
#1386=CIRCLE('',#3959,0.05);
#1387=CIRCLE('',#3961,0.0500000000000001);
#1388=CIRCLE('',#3963,0.0500000000000001);
#1389=CIRCLE('',#3965,0.0499999999999999);
#1390=CIRCLE('',#3967,0.0499999999999998);
#1391=CIRCLE('',#3969,0.0499999999999999);
#1392=CIRCLE('',#3971,0.0500000000000001);
#1393=CIRCLE('',#3973,0.0500000000000001);
#1394=CIRCLE('',#3975,0.0500000000000001);
#1395=CIRCLE('',#3977,0.0500000000000001);
#1396=CIRCLE('',#3979,0.0500000000000002);
#1397=CIRCLE('',#3980,0.05);
#1398=CIRCLE('',#3982,0.0500000000000001);
#1399=CIRCLE('',#3984,0.0500000000000002);
#1400=CIRCLE('',#3986,0.05);
#1401=CIRCLE('',#3987,0.0500000000000002);
#1402=CIRCLE('',#3989,0.0499999999999999);
#1403=CIRCLE('',#3991,0.05);
#1404=CIRCLE('',#3993,0.0500000000000002);
#1405=CIRCLE('',#3995,0.0499999999999999);
#1406=CIRCLE('',#3997,0.05);
#1407=CIRCLE('',#3999,0.05);
#1408=CIRCLE('',#4001,0.0499999999999999);
#1409=CIRCLE('',#4003,0.0499999999999999);
#1410=CIRCLE('',#4005,0.05);
#1411=CIRCLE('',#4007,0.05);
#1412=CIRCLE('',#4009,0.0500000000000001);
#1413=CIRCLE('',#4014,1.);
#1414=CIRCLE('',#4015,1.5);
#1415=CIRCLE('',#4018,0.175);
#1416=CIRCLE('',#4019,5.375);
#1417=CIRCLE('',#4021,0.175);
#1418=CIRCLE('',#4022,3.00073472959676);
#1419=CIRCLE('',#4024,0.175);
#1420=CIRCLE('',#4025,0.175);
#1421=VERTEX_POINT('',#5236);
#1422=VERTEX_POINT('',#5238);
#1423=VERTEX_POINT('',#5242);
#1424=VERTEX_POINT('',#5244);
#1425=VERTEX_POINT('',#5248);
#1426=VERTEX_POINT('',#5250);
#1427=VERTEX_POINT('',#5254);
#1428=VERTEX_POINT('',#5255);
#1429=VERTEX_POINT('',#5257);
#1430=VERTEX_POINT('',#5259);
#1431=VERTEX_POINT('',#5263);
#1432=VERTEX_POINT('',#5264);
#1433=VERTEX_POINT('',#5266);
#1434=VERTEX_POINT('',#5268);
#1435=VERTEX_POINT('',#5272);
#1436=VERTEX_POINT('',#5273);
#1437=VERTEX_POINT('',#5275);
#1438=VERTEX_POINT('',#5277);
#1439=VERTEX_POINT('',#5281);
#1440=VERTEX_POINT('',#5282);
#1441=VERTEX_POINT('',#5284);
#1442=VERTEX_POINT('',#5286);
#1443=VERTEX_POINT('',#5290);
#1444=VERTEX_POINT('',#5292);
#1445=VERTEX_POINT('',#5295);
#1446=VERTEX_POINT('',#5297);
#1447=VERTEX_POINT('',#5301);
#1448=VERTEX_POINT('',#5302);
#1449=VERTEX_POINT('',#5304);
#1450=VERTEX_POINT('',#5306);
#1451=VERTEX_POINT('',#5310);
#1452=VERTEX_POINT('',#5311);
#1453=VERTEX_POINT('',#5314);
#1454=VERTEX_POINT('',#5316);
#1455=VERTEX_POINT('',#5323);
#1456=VERTEX_POINT('',#5325);
#1457=VERTEX_POINT('',#5327);
#1458=VERTEX_POINT('',#5329);
#1459=VERTEX_POINT('',#5334);
#1460=VERTEX_POINT('',#5336);
#1461=VERTEX_POINT('',#5338);
#1462=VERTEX_POINT('',#5340);
#1463=VERTEX_POINT('',#5345);
#1464=VERTEX_POINT('',#5347);
#1465=VERTEX_POINT('',#5355);
#1466=VERTEX_POINT('',#5356);
#1467=VERTEX_POINT('',#5377);
#1468=VERTEX_POINT('',#5379);
#1469=VERTEX_POINT('',#5383);
#1470=VERTEX_POINT('',#5385);
#1471=VERTEX_POINT('',#5389);
#1472=VERTEX_POINT('',#5391);
#1473=VERTEX_POINT('',#5396);
#1474=VERTEX_POINT('',#5397);
#1475=VERTEX_POINT('',#5399);
#1476=VERTEX_POINT('',#5401);
#1477=VERTEX_POINT('',#5405);
#1478=VERTEX_POINT('',#5406);
#1479=VERTEX_POINT('',#5408);
#1480=VERTEX_POINT('',#5410);
#1481=VERTEX_POINT('',#5414);
#1482=VERTEX_POINT('',#5415);
#1483=VERTEX_POINT('',#5417);
#1484=VERTEX_POINT('',#5419);
#1485=VERTEX_POINT('',#5423);
#1486=VERTEX_POINT('',#5424);
#1487=VERTEX_POINT('',#5426);
#1488=VERTEX_POINT('',#5428);
#1489=VERTEX_POINT('',#5442);
#1490=VERTEX_POINT('',#5443);
#1491=VERTEX_POINT('',#5445);
#1492=VERTEX_POINT('',#5447);
#1493=VERTEX_POINT('',#5451);
#1494=VERTEX_POINT('',#5452);
#1495=VERTEX_POINT('',#5454);
#1496=VERTEX_POINT('',#5456);
#1497=VERTEX_POINT('',#5460);
#1498=VERTEX_POINT('',#5461);
#1499=VERTEX_POINT('',#5463);
#1500=VERTEX_POINT('',#5465);
#1501=VERTEX_POINT('',#5469);
#1502=VERTEX_POINT('',#5470);
#1503=VERTEX_POINT('',#5472);
#1504=VERTEX_POINT('',#5474);
#1505=VERTEX_POINT('',#5497);
#1506=VERTEX_POINT('',#5499);
#1507=VERTEX_POINT('',#5503);
#1508=VERTEX_POINT('',#5505);
#1509=VERTEX_POINT('',#5512);
#1510=VERTEX_POINT('',#5514);
#1511=VERTEX_POINT('',#5518);
#1512=VERTEX_POINT('',#5519);
#1513=VERTEX_POINT('',#5521);
#1514=VERTEX_POINT('',#5523);
#1515=VERTEX_POINT('',#5527);
#1516=VERTEX_POINT('',#5528);
#1517=VERTEX_POINT('',#5530);
#1518=VERTEX_POINT('',#5532);
#1519=VERTEX_POINT('',#5536);
#1520=VERTEX_POINT('',#5537);
#1521=VERTEX_POINT('',#5539);
#1522=VERTEX_POINT('',#5541);
#1523=VERTEX_POINT('',#5545);
#1524=VERTEX_POINT('',#5546);
#1525=VERTEX_POINT('',#5548);
#1526=VERTEX_POINT('',#5550);
#1527=VERTEX_POINT('',#5554);
#1528=VERTEX_POINT('',#5557);
#1529=VERTEX_POINT('',#5560);
#1530=VERTEX_POINT('',#5563);
#1531=VERTEX_POINT('',#5567);
#1532=VERTEX_POINT('',#5570);
#1533=VERTEX_POINT('',#5573);
#1534=VERTEX_POINT('',#5576);
#1535=VERTEX_POINT('',#6084);
#1536=VERTEX_POINT('',#6085);
#1537=VERTEX_POINT('',#6108);
#1538=VERTEX_POINT('',#6110);
#1539=VERTEX_POINT('',#6115);
#1540=VERTEX_POINT('',#6633);
#1541=VERTEX_POINT('',#6634);
#1542=VERTEX_POINT('',#6657);
#1543=VERTEX_POINT('',#6659);
#1544=VERTEX_POINT('',#6664);
#1545=VERTEX_POINT('',#6691);
#1546=VERTEX_POINT('',#6692);
#1547=VERTEX_POINT('',#6694);
#1548=VERTEX_POINT('',#6696);
#1549=VERTEX_POINT('',#6698);
#1550=VERTEX_POINT('',#6700);
#1551=VERTEX_POINT('',#6702);
#1552=VERTEX_POINT('',#6705);
#1553=VERTEX_POINT('',#6707);
#1554=VERTEX_POINT('',#6709);
#1555=VERTEX_POINT('',#6757);
#1556=VERTEX_POINT('',#6783);
#1557=VERTEX_POINT('',#6809);
#1558=VERTEX_POINT('',#6811);
#1559=VERTEX_POINT('',#6815);
#1560=VERTEX_POINT('',#6817);
#1561=VERTEX_POINT('',#6821);
#1562=VERTEX_POINT('',#6825);
#1563=VERTEX_POINT('',#6827);
#1564=VERTEX_POINT('',#6831);
#1565=VERTEX_POINT('',#6833);
#1566=VERTEX_POINT('',#6837);
#1567=VERTEX_POINT('',#6839);
#1568=VERTEX_POINT('',#7843);
#1569=VERTEX_POINT('',#7844);
#1570=VERTEX_POINT('',#7846);
#1571=VERTEX_POINT('',#7848);
#1572=VERTEX_POINT('',#7852);
#1573=VERTEX_POINT('',#7853);
#1574=VERTEX_POINT('',#7855);
#1575=VERTEX_POINT('',#7857);
#1576=VERTEX_POINT('',#7861);
#1577=VERTEX_POINT('',#7863);
#1578=VERTEX_POINT('',#7867);
#1579=VERTEX_POINT('',#7870);
#1580=VERTEX_POINT('',#7872);
#1581=VERTEX_POINT('',#7876);
#1582=VERTEX_POINT('',#7879);
#1583=VERTEX_POINT('',#7881);
#1584=VERTEX_POINT('',#7894);
#1585=VERTEX_POINT('',#7896);
#1586=VERTEX_POINT('',#7900);
#1587=VERTEX_POINT('',#7904);
#1588=VERTEX_POINT('',#7905);
#1589=VERTEX_POINT('',#7907);
#1590=VERTEX_POINT('',#7909);
#1591=VERTEX_POINT('',#7913);
#1592=VERTEX_POINT('',#7914);
#1593=VERTEX_POINT('',#7916);
#1594=VERTEX_POINT('',#7918);
#1595=VERTEX_POINT('',#7922);
#1596=VERTEX_POINT('',#7923);
#1597=VERTEX_POINT('',#7925);
#1598=VERTEX_POINT('',#7927);
#1599=VERTEX_POINT('',#7931);
#1600=VERTEX_POINT('',#7933);
#1601=VERTEX_POINT('',#7936);
#1602=VERTEX_POINT('',#7940);
#1603=VERTEX_POINT('',#7941);
#1604=VERTEX_POINT('',#7943);
#1605=VERTEX_POINT('',#7947);
#1606=VERTEX_POINT('',#7948);
#1607=VERTEX_POINT('',#7950);
#1608=VERTEX_POINT('',#7954);
#1609=VERTEX_POINT('',#7955);
#1610=VERTEX_POINT('',#7957);
#1611=VERTEX_POINT('',#7961);
#1612=VERTEX_POINT('',#7962);
#1613=VERTEX_POINT('',#7964);
#1614=VERTEX_POINT('',#7968);
#1615=VERTEX_POINT('',#7969);
#1616=VERTEX_POINT('',#7971);
#1617=VERTEX_POINT('',#7973);
#1618=VERTEX_POINT('',#7975);
#1619=VERTEX_POINT('',#7977);
#1620=VERTEX_POINT('',#7979);
#1621=VERTEX_POINT('',#7981);
#1622=VERTEX_POINT('',#7985);
#1623=VERTEX_POINT('',#7986);
#1624=VERTEX_POINT('',#7988);
#1625=VERTEX_POINT('',#7990);
#1626=VERTEX_POINT('',#7992);
#1627=VERTEX_POINT('',#7994);
#1628=VERTEX_POINT('',#7996);
#1629=VERTEX_POINT('',#7998);
#1630=VERTEX_POINT('',#8002);
#1631=VERTEX_POINT('',#8003);
#1632=VERTEX_POINT('',#8005);
#1633=VERTEX_POINT('',#8007);
#1634=VERTEX_POINT('',#8009);
#1635=VERTEX_POINT('',#8011);
#1636=VERTEX_POINT('',#8013);
#1637=VERTEX_POINT('',#8015);
#1638=VERTEX_POINT('',#8019);
#1639=VERTEX_POINT('',#8020);
#1640=VERTEX_POINT('',#8022);
#1641=VERTEX_POINT('',#8024);
#1642=VERTEX_POINT('',#8026);
#1643=VERTEX_POINT('',#8028);
#1644=VERTEX_POINT('',#8030);
#1645=VERTEX_POINT('',#8032);
#1646=VERTEX_POINT('',#8036);
#1647=VERTEX_POINT('',#8038);
#1648=VERTEX_POINT('',#8040);
#1649=VERTEX_POINT('',#8042);
#1650=VERTEX_POINT('',#8044);
#1651=VERTEX_POINT('',#8046);
#1652=VERTEX_POINT('',#8050);
#1653=VERTEX_POINT('',#8051);
#1654=VERTEX_POINT('',#8053);
#1655=VERTEX_POINT('',#8056);
#1656=VERTEX_POINT('',#8058);
#1657=VERTEX_POINT('',#8060);
#1658=VERTEX_POINT('',#8064);
#1659=VERTEX_POINT('',#8065);
#1660=VERTEX_POINT('',#8067);
#1661=VERTEX_POINT('',#8069);
#1662=VERTEX_POINT('',#8072);
#1663=VERTEX_POINT('',#8074);
#1664=VERTEX_POINT('',#8076);
#1665=VERTEX_POINT('',#8078);
#1666=VERTEX_POINT('',#8080);
#1667=VERTEX_POINT('',#8082);
#1668=VERTEX_POINT('',#8086);
#1669=VERTEX_POINT('',#8087);
#1670=VERTEX_POINT('',#8089);
#1671=VERTEX_POINT('',#8092);
#1672=VERTEX_POINT('',#8094);
#1673=VERTEX_POINT('',#8096);
#1674=VERTEX_POINT('',#8098);
#1675=VERTEX_POINT('',#8100);
#1676=VERTEX_POINT('',#8102);
#1677=VERTEX_POINT('',#8104);
#1678=VERTEX_POINT('',#8108);
#1679=VERTEX_POINT('',#8112);
#1680=VERTEX_POINT('',#8113);
#1681=VERTEX_POINT('',#8115);
#1682=VERTEX_POINT('',#8119);
#1683=VERTEX_POINT('',#8120);
#1684=VERTEX_POINT('',#8122);
#1685=VERTEX_POINT('',#8126);
#1686=VERTEX_POINT('',#8127);
#1687=VERTEX_POINT('',#8141);
#1688=VERTEX_POINT('',#8156);
#1689=VERTEX_POINT('',#8160);
#1690=VERTEX_POINT('',#8161);
#1691=VERTEX_POINT('',#8163);
#1692=VERTEX_POINT('',#8167);
#1693=VERTEX_POINT('',#8168);
#1694=VERTEX_POINT('',#8170);
#1695=VERTEX_POINT('',#8174);
#1696=VERTEX_POINT('',#8175);
#1697=VERTEX_POINT('',#8177);
#1698=VERTEX_POINT('',#8365);
#1699=VERTEX_POINT('',#8370);
#1700=VERTEX_POINT('',#8374);
#1701=VERTEX_POINT('',#8377);
#1702=VERTEX_POINT('',#8378);
#1703=VERTEX_POINT('',#8387);
#1704=VERTEX_POINT('',#8424);
#1705=VERTEX_POINT('',#9346);
#1706=VERTEX_POINT('',#9477);
#1707=EDGE_CURVE('',#1421,#1421,#1155,.T.);
#1708=EDGE_CURVE('',#1421,#1422,#761,.T.);
#1709=EDGE_CURVE('',#1422,#1422,#1156,.T.);
#1710=EDGE_CURVE('',#1423,#1423,#1157,.T.);
#1711=EDGE_CURVE('',#1423,#1424,#762,.T.);
#1712=EDGE_CURVE('',#1424,#1424,#1158,.T.);
#1713=EDGE_CURVE('',#1425,#1425,#1159,.T.);
#1714=EDGE_CURVE('',#1425,#1426,#763,.T.);
#1715=EDGE_CURVE('',#1426,#1426,#1160,.T.);
#1716=EDGE_CURVE('',#1427,#1428,#764,.T.);
#1717=EDGE_CURVE('',#1428,#1429,#765,.T.);
#1718=EDGE_CURVE('',#1429,#1430,#766,.T.);
#1719=EDGE_CURVE('',#1427,#1430,#767,.T.);
#1720=EDGE_CURVE('',#1431,#1432,#768,.T.);
#1721=EDGE_CURVE('',#1431,#1433,#769,.T.);
#1722=EDGE_CURVE('',#1434,#1433,#770,.T.);
#1723=EDGE_CURVE('',#1432,#1434,#771,.T.);
#1724=EDGE_CURVE('',#1435,#1436,#772,.T.);
#1725=EDGE_CURVE('',#1437,#1436,#773,.T.);
#1726=EDGE_CURVE('',#1437,#1438,#774,.T.);
#1727=EDGE_CURVE('',#1438,#1435,#775,.T.);
#1728=EDGE_CURVE('',#1439,#1440,#776,.T.);
#1729=EDGE_CURVE('',#1441,#1439,#777,.T.);
#1730=EDGE_CURVE('',#1442,#1441,#778,.T.);
#1731=EDGE_CURVE('',#1442,#1440,#779,.T.);
#1732=EDGE_CURVE('',#1443,#1433,#780,.T.);
#1733=EDGE_CURVE('',#1444,#1443,#781,.T.);
#1734=EDGE_CURVE('',#1439,#1444,#782,.T.);
#1735=EDGE_CURVE('',#1440,#1445,#783,.T.);
#1736=EDGE_CURVE('',#1445,#1446,#784,.T.);
#1737=EDGE_CURVE('',#1434,#1446,#785,.T.);
#1738=EDGE_CURVE('',#1447,#1448,#786,.T.);
#1739=EDGE_CURVE('',#1447,#1449,#787,.T.);
#1740=EDGE_CURVE('',#1449,#1450,#788,.T.);
#1741=EDGE_CURVE('',#1450,#1448,#789,.T.);
#1742=EDGE_CURVE('',#1451,#1452,#790,.T.);
#1743=EDGE_CURVE('',#1452,#1428,#791,.T.);
#1744=EDGE_CURVE('',#1453,#1427,#792,.T.);
#1745=EDGE_CURVE('',#1453,#1454,#793,.T.);
#1746=EDGE_CURVE('',#1454,#1438,#794,.T.);
#1747=EDGE_CURVE('',#1437,#1451,#795,.T.);
#1748=EDGE_CURVE('',#1446,#1447,#1161,.T.);
#1749=EDGE_CURVE('',#1448,#1453,#1162,.T.);
#1750=EDGE_CURVE('',#1455,#1430,#796,.T.);
#1751=EDGE_CURVE('',#1455,#1456,#1163,.T.);
#1752=EDGE_CURVE('',#1457,#1456,#797,.T.);
#1753=EDGE_CURVE('',#1457,#1458,#1164,.T.);
#1754=EDGE_CURVE('',#1432,#1458,#798,.T.);
#1755=EDGE_CURVE('',#1449,#1445,#1165,.T.);
#1756=EDGE_CURVE('',#1442,#1459,#799,.T.);
#1757=EDGE_CURVE('',#1459,#1460,#1166,.T.);
#1758=EDGE_CURVE('',#1460,#1461,#800,.T.);
#1759=EDGE_CURVE('',#1461,#1462,#1167,.T.);
#1760=EDGE_CURVE('',#1462,#1435,#801,.T.);
#1761=EDGE_CURVE('',#1454,#1450,#1168,.T.);
#1762=EDGE_CURVE('',#1429,#1463,#802,.T.);
#1763=EDGE_CURVE('',#1463,#1464,#803,.T.);
#1764=EDGE_CURVE('',#1464,#1436,#804,.T.);
#1765=EDGE_CURVE('',#1462,#1455,#805,.T.);
#1766=EDGE_CURVE('',#1460,#1457,#806,.T.);
#1767=EDGE_CURVE('',#1456,#1461,#807,.T.);
#1768=EDGE_CURVE('',#1465,#1466,#808,.T.);
#1769=EDGE_CURVE('',#1466,#1431,#809,.T.);
#1770=EDGE_CURVE('',#1458,#1459,#810,.T.);
#1771=EDGE_CURVE('',#1441,#1465,#811,.T.);
#1772=EDGE_CURVE('',#1465,#1444,#812,.T.);
#1773=EDGE_CURVE('',#1466,#1443,#813,.T.);
#1774=EDGE_CURVE('',#1452,#1463,#814,.T.);
#1775=EDGE_CURVE('',#1451,#1464,#815,.T.);
#1776=EDGE_CURVE('',#1467,#1467,#1169,.T.);
#1777=EDGE_CURVE('',#1467,#1468,#816,.T.);
#1778=EDGE_CURVE('',#1468,#1468,#1170,.T.);
#1779=EDGE_CURVE('',#1469,#1469,#1171,.T.);
#1780=EDGE_CURVE('',#1469,#1470,#817,.T.);
#1781=EDGE_CURVE('',#1470,#1470,#1172,.T.);
#1782=EDGE_CURVE('',#1471,#1471,#1173,.T.);
#1783=EDGE_CURVE('',#1471,#1472,#818,.T.);
#1784=EDGE_CURVE('',#1472,#1472,#1174,.T.);
#1785=EDGE_CURVE('',#1473,#1474,#819,.T.);
#1786=EDGE_CURVE('',#1474,#1475,#820,.T.);
#1787=EDGE_CURVE('',#1476,#1475,#821,.T.);
#1788=EDGE_CURVE('',#1476,#1473,#822,.T.);
#1789=EDGE_CURVE('',#1477,#1478,#823,.T.);
#1790=EDGE_CURVE('',#1478,#1479,#824,.T.);
#1791=EDGE_CURVE('',#1480,#1479,#825,.T.);
#1792=EDGE_CURVE('',#1480,#1477,#826,.T.);
#1793=EDGE_CURVE('',#1481,#1482,#827,.T.);
#1794=EDGE_CURVE('',#1481,#1483,#828,.T.);
#1795=EDGE_CURVE('',#1483,#1484,#829,.T.);
#1796=EDGE_CURVE('',#1484,#1482,#830,.T.);
#1797=EDGE_CURVE('',#1485,#1486,#831,.T.);
#1798=EDGE_CURVE('',#1485,#1487,#832,.T.);
#1799=EDGE_CURVE('',#1487,#1488,#833,.T.);
#1800=EDGE_CURVE('',#1488,#1486,#834,.T.);
#1801=EDGE_CURVE('',#1479,#1481,#1175,.T.);
#1802=EDGE_CURVE('',#1482,#1485,#1176,.T.);
#1803=EDGE_CURVE('',#1486,#1476,#1177,.T.);
#1804=EDGE_CURVE('',#1475,#1480,#1178,.T.);
#1805=EDGE_CURVE('',#1483,#1478,#1179,.T.);
#1806=EDGE_CURVE('',#1477,#1474,#1180,.T.);
#1807=EDGE_CURVE('',#1473,#1488,#1181,.T.);
#1808=EDGE_CURVE('',#1487,#1484,#1182,.T.);
#1809=EDGE_CURVE('',#1489,#1490,#835,.T.);
#1810=EDGE_CURVE('',#1490,#1491,#836,.T.);
#1811=EDGE_CURVE('',#1492,#1491,#837,.T.);
#1812=EDGE_CURVE('',#1492,#1489,#838,.T.);
#1813=EDGE_CURVE('',#1493,#1494,#839,.T.);
#1814=EDGE_CURVE('',#1494,#1495,#840,.T.);
#1815=EDGE_CURVE('',#1496,#1495,#841,.T.);
#1816=EDGE_CURVE('',#1496,#1493,#842,.T.);
#1817=EDGE_CURVE('',#1497,#1498,#843,.T.);
#1818=EDGE_CURVE('',#1497,#1499,#844,.T.);
#1819=EDGE_CURVE('',#1499,#1500,#845,.T.);
#1820=EDGE_CURVE('',#1500,#1498,#846,.T.);
#1821=EDGE_CURVE('',#1501,#1502,#847,.T.);
#1822=EDGE_CURVE('',#1501,#1503,#848,.T.);
#1823=EDGE_CURVE('',#1503,#1504,#849,.T.);
#1824=EDGE_CURVE('',#1504,#1502,#850,.T.);
#1825=EDGE_CURVE('',#1503,#1490,#1183,.T.);
#1826=EDGE_CURVE('',#1489,#1494,#1184,.T.);
#1827=EDGE_CURVE('',#1493,#1500,#1185,.T.);
#1828=EDGE_CURVE('',#1499,#1504,#1186,.T.);
#1829=EDGE_CURVE('',#1491,#1501,#1187,.T.);
#1830=EDGE_CURVE('',#1502,#1497,#1188,.T.);
#1831=EDGE_CURVE('',#1498,#1496,#1189,.T.);
#1832=EDGE_CURVE('',#1495,#1492,#1190,.T.);
#1833=EDGE_CURVE('',#1505,#1505,#1191,.T.);
#1834=EDGE_CURVE('',#1505,#1506,#851,.T.);
#1835=EDGE_CURVE('',#1506,#1506,#1192,.T.);
#1836=EDGE_CURVE('',#1507,#1507,#1193,.T.);
#1837=EDGE_CURVE('',#1507,#1508,#852,.T.);
#1838=EDGE_CURVE('',#1508,#1508,#1194,.T.);
#1839=EDGE_CURVE('',#1509,#1509,#1195,.T.);
#1840=EDGE_CURVE('',#1509,#1510,#853,.T.);
#1841=EDGE_CURVE('',#1510,#1510,#1196,.T.);
#1842=EDGE_CURVE('',#1511,#1512,#854,.T.);
#1843=EDGE_CURVE('',#1513,#1511,#855,.T.);
#1844=EDGE_CURVE('',#1513,#1514,#856,.T.);
#1845=EDGE_CURVE('',#1514,#1512,#857,.T.);
#1846=EDGE_CURVE('',#1515,#1516,#858,.T.);
#1847=EDGE_CURVE('',#1517,#1515,#859,.T.);
#1848=EDGE_CURVE('',#1517,#1518,#860,.T.);
#1849=EDGE_CURVE('',#1518,#1516,#861,.T.);
#1850=EDGE_CURVE('',#1519,#1520,#862,.T.);
#1851=EDGE_CURVE('',#1521,#1519,#863,.T.);
#1852=EDGE_CURVE('',#1521,#1522,#864,.T.);
#1853=EDGE_CURVE('',#1522,#1520,#865,.T.);
#1854=EDGE_CURVE('',#1523,#1524,#866,.T.);
#1855=EDGE_CURVE('',#1524,#1525,#867,.T.);
#1856=EDGE_CURVE('',#1526,#1525,#868,.T.);
#1857=EDGE_CURVE('',#1523,#1526,#869,.T.);
#1858=EDGE_CURVE('',#1527,#1525,#870,.T.);
#1859=EDGE_CURVE('',#1511,#1527,#871,.T.);
#1860=EDGE_CURVE('',#1528,#1512,#872,.T.);
#1861=EDGE_CURVE('',#1515,#1528,#873,.T.);
#1862=EDGE_CURVE('',#1529,#1516,#874,.T.);
#1863=EDGE_CURVE('',#1519,#1529,#875,.T.);
#1864=EDGE_CURVE('',#1530,#1520,#876,.T.);
#1865=EDGE_CURVE('',#1526,#1530,#877,.T.);
#1866=EDGE_CURVE('',#1531,#1513,#878,.T.);
#1867=EDGE_CURVE('',#1524,#1531,#879,.T.);
#1868=EDGE_CURVE('',#1532,#1523,#880,.T.);
#1869=EDGE_CURVE('',#1522,#1532,#881,.T.);
#1870=EDGE_CURVE('',#1533,#1521,#882,.T.);
#1871=EDGE_CURVE('',#1518,#1533,#883,.T.);
#1872=EDGE_CURVE('',#1534,#1517,#884,.T.);
#1873=EDGE_CURVE('',#1514,#1534,#885,.T.);
#1874=EDGE_CURVE('',#1532,#1530,#886,.T.);
#1875=EDGE_CURVE('',#1533,#1529,#887,.T.);
#1876=EDGE_CURVE('',#1534,#1528,#888,.T.);
#1877=EDGE_CURVE('',#1531,#1527,#889,.T.);
#1878=EDGE_CURVE('',#1535,#1536,#138,.T.);
#1879=EDGE_CURVE('',#1535,#1537,#890,.T.);
#1880=EDGE_CURVE('',#1538,#1537,#139,.F.);
#1881=EDGE_CURVE('',#1539,#1538,#140,.F.);
#1882=EDGE_CURVE('',#1536,#1539,#891,.T.);
#1883=EDGE_CURVE('',#1540,#1541,#141,.T.);
#1884=EDGE_CURVE('',#1540,#1542,#892,.T.);
#1885=EDGE_CURVE('',#1543,#1542,#142,.F.);
#1886=EDGE_CURVE('',#1544,#1543,#143,.F.);
#1887=EDGE_CURVE('',#1541,#1544,#893,.T.);
#1888=EDGE_CURVE('',#1545,#1546,#1197,.T.);
#1889=EDGE_CURVE('',#1546,#1547,#894,.T.);
#1890=EDGE_CURVE('',#1548,#1547,#1198,.T.);
#1891=EDGE_CURVE('',#1548,#1549,#895,.T.);
#1892=EDGE_CURVE('',#1549,#1550,#1199,.T.);
#1893=EDGE_CURVE('',#1550,#1551,#896,.T.);
#1894=EDGE_CURVE('',#1551,#1551,#1200,.T.);
#1895=EDGE_CURVE('',#1550,#1552,#1201,.T.);
#1896=EDGE_CURVE('',#1552,#1553,#897,.T.);
#1897=EDGE_CURVE('',#1554,#1553,#1202,.T.);
#1898=EDGE_CURVE('',#1554,#1545,#898,.T.);
#1899=EDGE_CURVE('',#1536,#1535,#144,.T.);
#1900=EDGE_CURVE('',#1541,#1540,#145,.T.);
#1901=EDGE_CURVE('',#1538,#1555,#899,.T.);
#1902=EDGE_CURVE('',#1555,#1555,#1203,.T.);
#1903=EDGE_CURVE('',#1537,#1539,#146,.T.);
#1904=EDGE_CURVE('',#1556,#1556,#1204,.T.);
#1905=EDGE_CURVE('',#1556,#1543,#900,.T.);
#1906=EDGE_CURVE('',#1542,#1544,#147,.T.);
#1907=EDGE_CURVE('',#1557,#1557,#1205,.T.);
#1908=EDGE_CURVE('',#1557,#1558,#901,.T.);
#1909=EDGE_CURVE('',#1558,#1558,#1206,.T.);
#1910=EDGE_CURVE('',#1559,#1559,#1207,.T.);
#1911=EDGE_CURVE('',#1559,#1560,#902,.T.);
#1912=EDGE_CURVE('',#1560,#1560,#1208,.T.);
#1913=EDGE_CURVE('',#1561,#1561,#1209,.T.);
#1914=EDGE_CURVE('',#1561,#1559,#903,.T.);
#1915=EDGE_CURVE('',#1562,#1562,#1210,.T.);
#1916=EDGE_CURVE('',#1562,#1563,#904,.T.);
#1917=EDGE_CURVE('',#1563,#1563,#1211,.T.);
#1918=EDGE_CURVE('',#1564,#1564,#1212,.T.);
#1919=EDGE_CURVE('',#1564,#1565,#905,.T.);
#1920=EDGE_CURVE('',#1565,#1565,#1213,.T.);
#1921=EDGE_CURVE('',#1566,#1566,#1214,.T.);
#1922=EDGE_CURVE('',#1566,#1567,#906,.T.);
#1923=EDGE_CURVE('',#1567,#1567,#1215,.T.);
#1924=EDGE_CURVE('',#1554,#1553,#907,.T.);
#1925=EDGE_CURVE('',#1545,#1552,#908,.T.);
#1926=EDGE_CURVE('',#1546,#1549,#909,.T.);
#1927=EDGE_CURVE('',#1547,#1548,#910,.T.);
#1928=EDGE_CURVE('',#1568,#1569,#1216,.T.);
#1929=EDGE_CURVE('',#1570,#1568,#911,.T.);
#1930=EDGE_CURVE('',#1571,#1570,#1217,.T.);
#1931=EDGE_CURVE('',#1569,#1571,#912,.T.);
#1932=EDGE_CURVE('',#1572,#1573,#1218,.T.);
#1933=EDGE_CURVE('',#1573,#1574,#913,.T.);
#1934=EDGE_CURVE('',#1574,#1575,#1219,.T.);
#1935=EDGE_CURVE('',#1572,#1575,#914,.T.);
#1936=EDGE_CURVE('',#1576,#1571,#1220,.T.);
#1937=EDGE_CURVE('',#1576,#1577,#915,.T.);
#1938=EDGE_CURVE('',#1577,#1569,#1221,.T.);
#1939=EDGE_CURVE('',#1578,#1574,#1222,.T.);
#1940=EDGE_CURVE('',#1578,#1576,#1223,.T.);
#1941=EDGE_CURVE('',#1579,#1570,#1224,.T.);
#1942=EDGE_CURVE('',#1580,#1579,#1225,.T.);
#1943=EDGE_CURVE('',#1575,#1580,#1226,.T.);
#1944=EDGE_CURVE('',#1577,#1581,#1227,.T.);
#1945=EDGE_CURVE('',#1573,#1581,#1228,.T.);
#1946=EDGE_CURVE('',#1582,#1572,#1229,.T.);
#1947=EDGE_CURVE('',#1583,#1582,#1230,.T.);
#1948=EDGE_CURVE('',#1568,#1583,#1231,.T.);
#1949=EDGE_CURVE('',#1582,#1580,#916,.T.);
#1950=EDGE_CURVE('',#1583,#1579,#917,.T.);
#1951=EDGE_CURVE('',#1581,#1578,#918,.T.);
#1952=EDGE_CURVE('',#1584,#1584,#1232,.T.);
#1953=EDGE_CURVE('',#1584,#1585,#919,.T.);
#1954=EDGE_CURVE('',#1585,#1585,#1233,.T.);
#1955=EDGE_CURVE('',#1586,#1586,#1234,.T.);
#1956=EDGE_CURVE('',#1586,#1584,#920,.T.);
#1957=EDGE_CURVE('',#1587,#1588,#1235,.T.);
#1958=EDGE_CURVE('',#1587,#1589,#1236,.T.);
#1959=EDGE_CURVE('',#1590,#1589,#1237,.T.);
#1960=EDGE_CURVE('',#1588,#1590,#1238,.T.);
#1961=EDGE_CURVE('',#1591,#1592,#1239,.T.);
#1962=EDGE_CURVE('',#1593,#1592,#921,.T.);
#1963=EDGE_CURVE('',#1594,#1593,#1240,.T.);
#1964=EDGE_CURVE('',#1591,#1594,#922,.T.);
#1965=EDGE_CURVE('',#1595,#1596,#1241,.T.);
#1966=EDGE_CURVE('',#1595,#1597,#1242,.T.);
#1967=EDGE_CURVE('',#1598,#1597,#1243,.T.);
#1968=EDGE_CURVE('',#1596,#1598,#1244,.T.);
#1969=EDGE_CURVE('',#1599,#1599,#1245,.T.);
#1970=EDGE_CURVE('',#1600,#1599,#1246,.T.);
#1971=EDGE_CURVE('',#1601,#1601,#1247,.T.);
#1972=EDGE_CURVE('',#1601,#1599,#923,.T.);
#1973=EDGE_CURVE('',#1602,#1603,#1248,.T.);
#1974=EDGE_CURVE('',#1603,#1604,#1249,.T.);
#1975=EDGE_CURVE('',#1604,#1602,#1250,.T.);
#1976=EDGE_CURVE('',#1605,#1606,#1251,.T.);
#1977=EDGE_CURVE('',#1606,#1607,#1252,.T.);
#1978=EDGE_CURVE('',#1607,#1605,#1253,.T.);
#1979=EDGE_CURVE('',#1608,#1609,#1254,.T.);
#1980=EDGE_CURVE('',#1609,#1610,#1255,.T.);
#1981=EDGE_CURVE('',#1610,#1608,#1256,.T.);
#1982=EDGE_CURVE('',#1611,#1612,#1257,.T.);
#1983=EDGE_CURVE('',#1612,#1613,#1258,.T.);
#1984=EDGE_CURVE('',#1613,#1611,#1259,.T.);
#1985=EDGE_CURVE('',#1614,#1615,#924,.T.);
#1986=EDGE_CURVE('',#1615,#1616,#1260,.T.);
#1987=EDGE_CURVE('',#1616,#1617,#925,.T.);
#1988=EDGE_CURVE('',#1617,#1618,#1261,.T.);
#1989=EDGE_CURVE('',#1618,#1619,#926,.T.);
#1990=EDGE_CURVE('',#1619,#1620,#1262,.T.);
#1991=EDGE_CURVE('',#1620,#1621,#927,.T.);
#1992=EDGE_CURVE('',#1621,#1614,#1263,.T.);
#1993=EDGE_CURVE('',#1622,#1623,#1264,.T.);
#1994=EDGE_CURVE('',#1623,#1624,#928,.T.);
#1995=EDGE_CURVE('',#1624,#1625,#1265,.T.);
#1996=EDGE_CURVE('',#1625,#1626,#929,.T.);
#1997=EDGE_CURVE('',#1626,#1627,#1266,.T.);
#1998=EDGE_CURVE('',#1627,#1628,#930,.T.);
#1999=EDGE_CURVE('',#1628,#1629,#1267,.T.);
#2000=EDGE_CURVE('',#1629,#1622,#931,.T.);
#2001=EDGE_CURVE('',#1630,#1631,#1268,.T.);
#2002=EDGE_CURVE('',#1631,#1632,#932,.T.);
#2003=EDGE_CURVE('',#1632,#1633,#1269,.T.);
#2004=EDGE_CURVE('',#1633,#1634,#933,.T.);
#2005=EDGE_CURVE('',#1634,#1635,#1270,.T.);
#2006=EDGE_CURVE('',#1635,#1636,#934,.T.);
#2007=EDGE_CURVE('',#1636,#1637,#1271,.T.);
#2008=EDGE_CURVE('',#1637,#1630,#935,.T.);
#2009=EDGE_CURVE('',#1638,#1639,#1272,.T.);
#2010=EDGE_CURVE('',#1639,#1640,#936,.T.);
#2011=EDGE_CURVE('',#1640,#1641,#1273,.T.);
#2012=EDGE_CURVE('',#1641,#1642,#937,.T.);
#2013=EDGE_CURVE('',#1642,#1643,#1274,.T.);
#2014=EDGE_CURVE('',#1643,#1644,#938,.T.);
#2015=EDGE_CURVE('',#1644,#1645,#1275,.T.);
#2016=EDGE_CURVE('',#1645,#1638,#939,.T.);
#2017=EDGE_CURVE('',#1592,#1646,#1276,.T.);
#2018=EDGE_CURVE('',#1646,#1647,#940,.T.);
#2019=EDGE_CURVE('',#1647,#1648,#1277,.T.);
#2020=EDGE_CURVE('',#1648,#1649,#941,.T.);
#2021=EDGE_CURVE('',#1649,#1650,#1278,.T.);
#2022=EDGE_CURVE('',#1650,#1651,#942,.T.);
#2023=EDGE_CURVE('',#1651,#1593,#1279,.T.);
#2024=EDGE_CURVE('',#1652,#1653,#1280,.T.);
#2025=EDGE_CURVE('',#1653,#1654,#943,.T.);
#2026=EDGE_CURVE('',#1654,#1591,#1281,.T.);
#2027=EDGE_CURVE('',#1594,#1655,#1282,.T.);
#2028=EDGE_CURVE('',#1655,#1656,#944,.T.);
#2029=EDGE_CURVE('',#1656,#1657,#1283,.T.);
#2030=EDGE_CURVE('',#1657,#1652,#945,.T.);
#2031=EDGE_CURVE('',#1658,#1659,#1284,.T.);
#2032=EDGE_CURVE('',#1658,#1660,#946,.T.);
#2033=EDGE_CURVE('',#1660,#1661,#1285,.T.);
#2034=EDGE_CURVE('',#1661,#1598,#947,.T.);
#2035=EDGE_CURVE('',#1597,#1662,#948,.T.);
#2036=EDGE_CURVE('',#1662,#1663,#1286,.T.);
#2037=EDGE_CURVE('',#1663,#1664,#949,.T.);
#2038=EDGE_CURVE('',#1664,#1665,#1287,.T.);
#2039=EDGE_CURVE('',#1665,#1666,#950,.T.);
#2040=EDGE_CURVE('',#1666,#1667,#1288,.T.);
#2041=EDGE_CURVE('',#1667,#1659,#951,.T.);
#2042=EDGE_CURVE('',#1668,#1669,#952,.T.);
#2043=EDGE_CURVE('',#1669,#1670,#1289,.T.);
#2044=EDGE_CURVE('',#1670,#1587,#953,.T.);
#2045=EDGE_CURVE('',#1588,#1671,#954,.T.);
#2046=EDGE_CURVE('',#1671,#1672,#1290,.T.);
#2047=EDGE_CURVE('',#1672,#1673,#955,.T.);
#2048=EDGE_CURVE('',#1673,#1674,#1291,.T.);
#2049=EDGE_CURVE('',#1674,#1675,#956,.T.);
#2050=EDGE_CURVE('',#1675,#1676,#1292,.T.);
#2051=EDGE_CURVE('',#1676,#1677,#957,.T.);
#2052=EDGE_CURVE('',#1677,#1668,#1293,.T.);
#2053=EDGE_CURVE('',#1596,#1678,#1294,.T.);
#2054=EDGE_CURVE('',#1678,#1595,#1295,.T.);
#2055=EDGE_CURVE('',#1679,#1680,#1296,.T.);
#2056=EDGE_CURVE('',#1680,#1681,#1297,.T.);
#2057=EDGE_CURVE('',#1681,#1679,#1298,.T.);
#2058=EDGE_CURVE('',#1682,#1683,#1299,.T.);
#2059=EDGE_CURVE('',#1683,#1684,#1300,.T.);
#2060=EDGE_CURVE('',#1684,#1682,#1301,.T.);
#2061=EDGE_CURVE('',#1685,#1686,#1302,.T.);
#2062=EDGE_CURVE('',#1686,#1658,#148,.T.);
#2063=EDGE_CURVE('',#1659,#1687,#149,.T.);
#2064=EDGE_CURVE('',#1687,#1685,#1303,.T.);
#2065=EDGE_CURVE('',#1589,#1688,#1304,.T.);
#2066=EDGE_CURVE('',#1688,#1590,#1305,.T.);
#2067=EDGE_CURVE('',#1689,#1690,#1306,.T.);
#2068=EDGE_CURVE('',#1690,#1691,#1307,.T.);
#2069=EDGE_CURVE('',#1691,#1689,#1308,.T.);
#2070=EDGE_CURVE('',#1692,#1693,#1309,.T.);
#2071=EDGE_CURVE('',#1693,#1694,#1310,.T.);
#2072=EDGE_CURVE('',#1694,#1692,#1311,.T.);
#2073=EDGE_CURVE('',#1695,#1696,#1312,.T.);
#2074=EDGE_CURVE('',#1696,#1697,#1313,.T.);
#2075=EDGE_CURVE('',#1697,#1695,#1314,.T.);
#2076=EDGE_CURVE('',#1640,#1681,#1315,.T.);
#2077=EDGE_CURVE('',#1663,#1640,#1316,.T.);
#2078=EDGE_CURVE('',#1681,#1663,#1317,.T.);
#2079=EDGE_CURVE('',#1664,#1639,#1318,.T.);
#2080=EDGE_CURVE('',#1679,#1662,#1319,.T.);
#2081=EDGE_CURVE('',#1680,#1634,#1320,.T.);
#2082=EDGE_CURVE('',#1635,#1679,#1321,.T.);
#2083=EDGE_CURVE('',#1641,#1680,#1322,.T.);
#2084=EDGE_CURVE('',#1639,#1612,#1323,.T.);
#2085=EDGE_CURVE('',#1613,#1638,#1324,.T.);
#2086=EDGE_CURVE('',#1664,#1612,#1325,.T.);
#2087=EDGE_CURVE('',#1635,#1662,#1326,.T.);
#2088=EDGE_CURVE('',#1641,#1634,#1327,.T.);
#2089=EDGE_CURVE('',#1648,#1638,#1328,.T.);
#2090=EDGE_CURVE('',#1613,#1648,#1329,.T.);
#2091=EDGE_CURVE('',#1611,#1647,#1330,.T.);
#2092=EDGE_CURVE('',#1665,#1611,#1331,.T.);
#2093=EDGE_CURVE('',#1636,#1597,#1332,.T.);
#2094=EDGE_CURVE('',#1642,#1633,#1333,.T.);
#2095=EDGE_CURVE('',#1643,#1690,#1334,.T.);
#2096=EDGE_CURVE('',#1691,#1642,#1335,.T.);
#2097=EDGE_CURVE('',#1644,#1668,#1336,.T.);
#2098=EDGE_CURVE('',#1669,#1643,#1337,.T.);
#2099=EDGE_CURVE('',#1645,#1607,#1338,.T.);
#2100=EDGE_CURVE('',#1605,#1644,#1339,.T.);
#2101=EDGE_CURVE('',#1649,#1645,#1340,.T.);
#2102=EDGE_CURVE('',#1665,#1647,#1341,.T.);
#2103=EDGE_CURVE('',#1636,#1595,#1342,.T.);
#2104=EDGE_CURVE('',#1691,#1633,#1343,.T.);
#2105=EDGE_CURVE('',#1669,#1690,#1344,.T.);
#2106=EDGE_CURVE('',#1605,#1668,#1345,.T.);
#2107=EDGE_CURVE('',#1649,#1607,#1346,.T.);
#2108=EDGE_CURVE('',#1666,#1646,#1347,.T.);
#2109=EDGE_CURVE('',#1678,#1626,#1348,.T.);
#2110=EDGE_CURVE('',#1627,#1596,#1349,.T.);
#2111=EDGE_CURVE('',#1637,#1678,#1350,.T.);
#2112=EDGE_CURVE('',#1689,#1632,#1351,.T.);
#2113=EDGE_CURVE('',#1670,#1689,#1352,.T.);
#2114=EDGE_CURVE('',#1606,#1677,#1353,.T.);
#2115=EDGE_CURVE('',#1650,#1606,#1354,.T.);
#2116=EDGE_CURVE('',#1646,#1682,#1355,.T.);
#2117=EDGE_CURVE('',#1683,#1592,#1356,.T.);
#2118=EDGE_CURVE('',#1666,#1682,#1357,.T.);
#2119=EDGE_CURVE('',#1627,#1598,#1358,.T.);
#2120=EDGE_CURVE('',#1637,#1626,#1359,.T.);
#2121=EDGE_CURVE('',#1670,#1632,#1360,.T.);
#2122=EDGE_CURVE('',#1650,#1677,#1361,.T.);
#2123=EDGE_CURVE('',#1683,#1591,#1362,.T.);
#2124=EDGE_CURVE('',#1684,#1654,#1363,.T.);
#2125=EDGE_CURVE('',#1667,#1684,#1364,.T.);
#2126=EDGE_CURVE('',#1661,#1608,#1365,.T.);
#2127=EDGE_CURVE('',#1609,#1660,#1366,.T.);
#2128=EDGE_CURVE('',#1628,#1661,#1367,.T.);
#2129=EDGE_CURVE('',#1630,#1625,#1368,.T.);
#2130=EDGE_CURVE('',#1631,#1589,#1369,.T.);
#2131=EDGE_CURVE('',#1688,#1630,#1370,.T.);
#2132=EDGE_CURVE('',#1587,#1631,#1371,.T.);
#2133=EDGE_CURVE('',#1651,#1676,#1372,.T.);
#2134=EDGE_CURVE('',#1593,#1694,#1373,.T.);
#2135=EDGE_CURVE('',#1692,#1651,#1374,.T.);
#2136=EDGE_CURVE('',#1667,#1654,#1375,.T.);
#2137=EDGE_CURVE('',#1609,#1620,#1376,.T.);
#2138=EDGE_CURVE('',#1620,#1660,#1377,.T.);
#2139=EDGE_CURVE('',#1628,#1608,#1378,.T.);
#2140=EDGE_CURVE('',#1688,#1625,#1379,.T.);
#2141=EDGE_CURVE('',#1692,#1676,#1380,.T.);
#2142=EDGE_CURVE('',#1594,#1694,#1381,.T.);
#2143=EDGE_CURVE('',#1687,#1653,#1382,.T.);
#2144=EDGE_CURVE('',#1621,#1686,#1383,.T.);
#2145=EDGE_CURVE('',#1610,#1619,#1384,.T.);
#2146=EDGE_CURVE('',#1629,#1610,#1385,.T.);
#2147=EDGE_CURVE('',#1590,#1624,#1386,.T.);
#2148=EDGE_CURVE('',#1693,#1675,#1387,.T.);
#2149=EDGE_CURVE('',#1655,#1693,#1388,.T.);
#2150=EDGE_CURVE('',#1685,#1652,#1389,.T.);
#2151=EDGE_CURVE('',#1614,#1685,#1390,.T.);
#2152=EDGE_CURVE('',#1629,#1619,#1391,.T.);
#2153=EDGE_CURVE('',#1588,#1624,#1392,.T.);
#2154=EDGE_CURVE('',#1655,#1675,#1393,.T.);
#2155=EDGE_CURVE('',#1614,#1652,#1394,.T.);
#2156=EDGE_CURVE('',#1622,#1618,#1395,.T.);
#2157=EDGE_CURVE('',#1623,#1603,#1396,.T.);
#2158=EDGE_CURVE('',#1604,#1622,#1397,.T.);
#2159=EDGE_CURVE('',#1671,#1623,#1398,.T.);
#2160=EDGE_CURVE('',#1656,#1674,#1399,.T.);
#2161=EDGE_CURVE('',#1657,#1697,#1400,.T.);
#2162=EDGE_CURVE('',#1695,#1656,#1401,.T.);
#2163=EDGE_CURVE('',#1615,#1657,#1402,.T.);
#2164=EDGE_CURVE('',#1604,#1618,#1403,.T.);
#2165=EDGE_CURVE('',#1671,#1603,#1404,.T.);
#2166=EDGE_CURVE('',#1695,#1674,#1405,.T.);
#2167=EDGE_CURVE('',#1615,#1697,#1406,.T.);
#2168=EDGE_CURVE('',#1602,#1617,#1407,.T.);
#2169=EDGE_CURVE('',#1672,#1602,#1408,.T.);
#2170=EDGE_CURVE('',#1696,#1673,#1409,.T.);
#2171=EDGE_CURVE('',#1616,#1696,#1410,.T.);
#2172=EDGE_CURVE('',#1672,#1617,#1411,.T.);
#2173=EDGE_CURVE('',#1616,#1673,#1412,.T.);
#2174=EDGE_CURVE('',#1698,#1698,#1413,.T.);
#2175=EDGE_CURVE('',#1698,#1698,#1414,.T.);
#2176=EDGE_CURVE('',#1699,#1699,#1415,.T.);
#2177=EDGE_CURVE('',#1699,#1699,#1416,.T.);
#2178=EDGE_CURVE('',#1700,#1700,#1417,.T.);
#2179=EDGE_CURVE('',#1700,#1700,#1418,.T.);
#2180=EDGE_CURVE('',#1701,#1702,#150,.F.);
#2181=EDGE_CURVE('',#1702,#1703,#151,.T.);
#2182=EDGE_CURVE('',#1703,#1704,#152,.T.);
#2183=EDGE_CURVE('',#1704,#1701,#49,.T.);
#2184=EDGE_CURVE('',#1703,#1705,#153,.T.);
#2185=EDGE_CURVE('',#1705,#1706,#1419,.T.);
#2186=EDGE_CURVE('',#1701,#1706,#154,.T.);
#2187=EDGE_CURVE('',#1706,#1705,#1420,.T.);
#2188=ORIENTED_EDGE('',*,*,#1707,.T.);
#2189=ORIENTED_EDGE('',*,*,#1708,.T.);
#2190=ORIENTED_EDGE('',*,*,#1709,.T.);
#2191=ORIENTED_EDGE('',*,*,#1708,.F.);
#2192=ORIENTED_EDGE('',*,*,#1710,.T.);
#2193=ORIENTED_EDGE('',*,*,#1711,.T.);
#2194=ORIENTED_EDGE('',*,*,#1712,.T.);
#2195=ORIENTED_EDGE('',*,*,#1711,.F.);
#2196=ORIENTED_EDGE('',*,*,#1713,.T.);
#2197=ORIENTED_EDGE('',*,*,#1714,.T.);
#2198=ORIENTED_EDGE('',*,*,#1715,.T.);
#2199=ORIENTED_EDGE('',*,*,#1714,.F.);
#2200=ORIENTED_EDGE('',*,*,#1716,.T.);
#2201=ORIENTED_EDGE('',*,*,#1717,.T.);
#2202=ORIENTED_EDGE('',*,*,#1718,.T.);
#2203=ORIENTED_EDGE('',*,*,#1719,.F.);
#2204=ORIENTED_EDGE('',*,*,#1720,.F.);
#2205=ORIENTED_EDGE('',*,*,#1721,.T.);
#2206=ORIENTED_EDGE('',*,*,#1722,.F.);
#2207=ORIENTED_EDGE('',*,*,#1723,.F.);
#2208=ORIENTED_EDGE('',*,*,#1724,.T.);
#2209=ORIENTED_EDGE('',*,*,#1725,.F.);
#2210=ORIENTED_EDGE('',*,*,#1726,.T.);
#2211=ORIENTED_EDGE('',*,*,#1727,.T.);
#2212=ORIENTED_EDGE('',*,*,#1728,.F.);
#2213=ORIENTED_EDGE('',*,*,#1729,.F.);
#2214=ORIENTED_EDGE('',*,*,#1730,.F.);
#2215=ORIENTED_EDGE('',*,*,#1731,.T.);
#2216=ORIENTED_EDGE('',*,*,#1722,.T.);
#2217=ORIENTED_EDGE('',*,*,#1732,.F.);
#2218=ORIENTED_EDGE('',*,*,#1733,.F.);
#2219=ORIENTED_EDGE('',*,*,#1734,.F.);
#2220=ORIENTED_EDGE('',*,*,#1728,.T.);
#2221=ORIENTED_EDGE('',*,*,#1735,.T.);
#2222=ORIENTED_EDGE('',*,*,#1736,.T.);
#2223=ORIENTED_EDGE('',*,*,#1737,.F.);
#2224=ORIENTED_EDGE('',*,*,#1709,.F.);
#2225=ORIENTED_EDGE('',*,*,#1712,.F.);
#2226=ORIENTED_EDGE('',*,*,#1738,.F.);
#2227=ORIENTED_EDGE('',*,*,#1739,.T.);
#2228=ORIENTED_EDGE('',*,*,#1740,.T.);
#2229=ORIENTED_EDGE('',*,*,#1741,.T.);
#2230=ORIENTED_EDGE('',*,*,#1715,.F.);
#2231=ORIENTED_EDGE('',*,*,#1742,.T.);
#2232=ORIENTED_EDGE('',*,*,#1743,.T.);
#2233=ORIENTED_EDGE('',*,*,#1716,.F.);
#2234=ORIENTED_EDGE('',*,*,#1744,.F.);
#2235=ORIENTED_EDGE('',*,*,#1745,.T.);
#2236=ORIENTED_EDGE('',*,*,#1746,.T.);
#2237=ORIENTED_EDGE('',*,*,#1726,.F.);
#2238=ORIENTED_EDGE('',*,*,#1747,.T.);
#2239=ORIENTED_EDGE('',*,*,#1737,.T.);
#2240=ORIENTED_EDGE('',*,*,#1748,.T.);
#2241=ORIENTED_EDGE('',*,*,#1738,.T.);
#2242=ORIENTED_EDGE('',*,*,#1749,.T.);
#2243=ORIENTED_EDGE('',*,*,#1744,.T.);
#2244=ORIENTED_EDGE('',*,*,#1719,.T.);
#2245=ORIENTED_EDGE('',*,*,#1750,.F.);
#2246=ORIENTED_EDGE('',*,*,#1751,.T.);
#2247=ORIENTED_EDGE('',*,*,#1752,.F.);
#2248=ORIENTED_EDGE('',*,*,#1753,.T.);
#2249=ORIENTED_EDGE('',*,*,#1754,.F.);
#2250=ORIENTED_EDGE('',*,*,#1723,.T.);
#2251=ORIENTED_EDGE('',*,*,#1740,.F.);
#2252=ORIENTED_EDGE('',*,*,#1755,.T.);
#2253=ORIENTED_EDGE('',*,*,#1735,.F.);
#2254=ORIENTED_EDGE('',*,*,#1731,.F.);
#2255=ORIENTED_EDGE('',*,*,#1756,.T.);
#2256=ORIENTED_EDGE('',*,*,#1757,.T.);
#2257=ORIENTED_EDGE('',*,*,#1758,.T.);
#2258=ORIENTED_EDGE('',*,*,#1759,.T.);
#2259=ORIENTED_EDGE('',*,*,#1760,.T.);
#2260=ORIENTED_EDGE('',*,*,#1727,.F.);
#2261=ORIENTED_EDGE('',*,*,#1746,.F.);
#2262=ORIENTED_EDGE('',*,*,#1761,.T.);
#2263=ORIENTED_EDGE('',*,*,#1718,.F.);
#2264=ORIENTED_EDGE('',*,*,#1762,.T.);
#2265=ORIENTED_EDGE('',*,*,#1763,.T.);
#2266=ORIENTED_EDGE('',*,*,#1764,.T.);
#2267=ORIENTED_EDGE('',*,*,#1724,.F.);
#2268=ORIENTED_EDGE('',*,*,#1760,.F.);
#2269=ORIENTED_EDGE('',*,*,#1765,.T.);
#2270=ORIENTED_EDGE('',*,*,#1750,.T.);
#2271=ORIENTED_EDGE('',*,*,#1758,.F.);
#2272=ORIENTED_EDGE('',*,*,#1766,.T.);
#2273=ORIENTED_EDGE('',*,*,#1752,.T.);
#2274=ORIENTED_EDGE('',*,*,#1767,.T.);
#2275=ORIENTED_EDGE('',*,*,#1713,.F.);
#2276=ORIENTED_EDGE('',*,*,#1768,.T.);
#2277=ORIENTED_EDGE('',*,*,#1769,.T.);
#2278=ORIENTED_EDGE('',*,*,#1720,.T.);
#2279=ORIENTED_EDGE('',*,*,#1754,.T.);
#2280=ORIENTED_EDGE('',*,*,#1770,.T.);
#2281=ORIENTED_EDGE('',*,*,#1756,.F.);
#2282=ORIENTED_EDGE('',*,*,#1730,.T.);
#2283=ORIENTED_EDGE('',*,*,#1771,.T.);
#2284=ORIENTED_EDGE('',*,*,#1707,.F.);
#2285=ORIENTED_EDGE('',*,*,#1710,.F.);
#2286=ORIENTED_EDGE('',*,*,#1748,.F.);
#2287=ORIENTED_EDGE('',*,*,#1736,.F.);
#2288=ORIENTED_EDGE('',*,*,#1755,.F.);
#2289=ORIENTED_EDGE('',*,*,#1739,.F.);
#2290=ORIENTED_EDGE('',*,*,#1749,.F.);
#2291=ORIENTED_EDGE('',*,*,#1741,.F.);
#2292=ORIENTED_EDGE('',*,*,#1761,.F.);
#2293=ORIENTED_EDGE('',*,*,#1745,.F.);
#2294=ORIENTED_EDGE('',*,*,#1757,.F.);
#2295=ORIENTED_EDGE('',*,*,#1770,.F.);
#2296=ORIENTED_EDGE('',*,*,#1753,.F.);
#2297=ORIENTED_EDGE('',*,*,#1766,.F.);
#2298=ORIENTED_EDGE('',*,*,#1759,.F.);
#2299=ORIENTED_EDGE('',*,*,#1767,.F.);
#2300=ORIENTED_EDGE('',*,*,#1751,.F.);
#2301=ORIENTED_EDGE('',*,*,#1765,.F.);
#2302=ORIENTED_EDGE('',*,*,#1729,.T.);
#2303=ORIENTED_EDGE('',*,*,#1734,.T.);
#2304=ORIENTED_EDGE('',*,*,#1772,.F.);
#2305=ORIENTED_EDGE('',*,*,#1771,.F.);
#2306=ORIENTED_EDGE('',*,*,#1772,.T.);
#2307=ORIENTED_EDGE('',*,*,#1733,.T.);
#2308=ORIENTED_EDGE('',*,*,#1773,.F.);
#2309=ORIENTED_EDGE('',*,*,#1768,.F.);
#2310=ORIENTED_EDGE('',*,*,#1773,.T.);
#2311=ORIENTED_EDGE('',*,*,#1732,.T.);
#2312=ORIENTED_EDGE('',*,*,#1721,.F.);
#2313=ORIENTED_EDGE('',*,*,#1769,.F.);
#2314=ORIENTED_EDGE('',*,*,#1717,.F.);
#2315=ORIENTED_EDGE('',*,*,#1743,.F.);
#2316=ORIENTED_EDGE('',*,*,#1774,.T.);
#2317=ORIENTED_EDGE('',*,*,#1762,.F.);
#2318=ORIENTED_EDGE('',*,*,#1774,.F.);
#2319=ORIENTED_EDGE('',*,*,#1742,.F.);
#2320=ORIENTED_EDGE('',*,*,#1775,.T.);
#2321=ORIENTED_EDGE('',*,*,#1763,.F.);
#2322=ORIENTED_EDGE('',*,*,#1775,.F.);
#2323=ORIENTED_EDGE('',*,*,#1747,.F.);
#2324=ORIENTED_EDGE('',*,*,#1725,.T.);
#2325=ORIENTED_EDGE('',*,*,#1764,.F.);
#2326=ORIENTED_EDGE('',*,*,#1776,.T.);
#2327=ORIENTED_EDGE('',*,*,#1777,.T.);
#2328=ORIENTED_EDGE('',*,*,#1778,.T.);
#2329=ORIENTED_EDGE('',*,*,#1777,.F.);
#2330=ORIENTED_EDGE('',*,*,#1779,.T.);
#2331=ORIENTED_EDGE('',*,*,#1780,.T.);
#2332=ORIENTED_EDGE('',*,*,#1781,.F.);
#2333=ORIENTED_EDGE('',*,*,#1780,.F.);
#2334=ORIENTED_EDGE('',*,*,#1782,.T.);
#2335=ORIENTED_EDGE('',*,*,#1783,.T.);
#2336=ORIENTED_EDGE('',*,*,#1784,.T.);
#2337=ORIENTED_EDGE('',*,*,#1783,.F.);
#2338=ORIENTED_EDGE('',*,*,#1784,.F.);
#2339=ORIENTED_EDGE('',*,*,#1778,.F.);
#2340=ORIENTED_EDGE('',*,*,#1785,.T.);
#2341=ORIENTED_EDGE('',*,*,#1786,.T.);
#2342=ORIENTED_EDGE('',*,*,#1787,.F.);
#2343=ORIENTED_EDGE('',*,*,#1788,.T.);
#2344=ORIENTED_EDGE('',*,*,#1789,.T.);
#2345=ORIENTED_EDGE('',*,*,#1790,.T.);
#2346=ORIENTED_EDGE('',*,*,#1791,.F.);
#2347=ORIENTED_EDGE('',*,*,#1792,.T.);
#2348=ORIENTED_EDGE('',*,*,#1793,.F.);
#2349=ORIENTED_EDGE('',*,*,#1794,.T.);
#2350=ORIENTED_EDGE('',*,*,#1795,.T.);
#2351=ORIENTED_EDGE('',*,*,#1796,.T.);
#2352=ORIENTED_EDGE('',*,*,#1797,.F.);
#2353=ORIENTED_EDGE('',*,*,#1798,.T.);
#2354=ORIENTED_EDGE('',*,*,#1799,.T.);
#2355=ORIENTED_EDGE('',*,*,#1800,.T.);
#2356=ORIENTED_EDGE('',*,*,#1791,.T.);
#2357=ORIENTED_EDGE('',*,*,#1801,.T.);
#2358=ORIENTED_EDGE('',*,*,#1793,.T.);
#2359=ORIENTED_EDGE('',*,*,#1802,.T.);
#2360=ORIENTED_EDGE('',*,*,#1797,.T.);
#2361=ORIENTED_EDGE('',*,*,#1803,.T.);
#2362=ORIENTED_EDGE('',*,*,#1787,.T.);
#2363=ORIENTED_EDGE('',*,*,#1804,.T.);
#2364=ORIENTED_EDGE('',*,*,#1782,.F.);
#2365=ORIENTED_EDGE('',*,*,#1795,.F.);
#2366=ORIENTED_EDGE('',*,*,#1805,.T.);
#2367=ORIENTED_EDGE('',*,*,#1789,.F.);
#2368=ORIENTED_EDGE('',*,*,#1806,.T.);
#2369=ORIENTED_EDGE('',*,*,#1785,.F.);
#2370=ORIENTED_EDGE('',*,*,#1807,.T.);
#2371=ORIENTED_EDGE('',*,*,#1799,.F.);
#2372=ORIENTED_EDGE('',*,*,#1808,.T.);
#2373=ORIENTED_EDGE('',*,*,#1781,.T.);
#2374=ORIENTED_EDGE('',*,*,#1809,.T.);
#2375=ORIENTED_EDGE('',*,*,#1810,.T.);
#2376=ORIENTED_EDGE('',*,*,#1811,.F.);
#2377=ORIENTED_EDGE('',*,*,#1812,.T.);
#2378=ORIENTED_EDGE('',*,*,#1813,.T.);
#2379=ORIENTED_EDGE('',*,*,#1814,.T.);
#2380=ORIENTED_EDGE('',*,*,#1815,.F.);
#2381=ORIENTED_EDGE('',*,*,#1816,.T.);
#2382=ORIENTED_EDGE('',*,*,#1817,.F.);
#2383=ORIENTED_EDGE('',*,*,#1818,.T.);
#2384=ORIENTED_EDGE('',*,*,#1819,.T.);
#2385=ORIENTED_EDGE('',*,*,#1820,.T.);
#2386=ORIENTED_EDGE('',*,*,#1821,.F.);
#2387=ORIENTED_EDGE('',*,*,#1822,.T.);
#2388=ORIENTED_EDGE('',*,*,#1823,.T.);
#2389=ORIENTED_EDGE('',*,*,#1824,.T.);
#2390=ORIENTED_EDGE('',*,*,#1823,.F.);
#2391=ORIENTED_EDGE('',*,*,#1825,.T.);
#2392=ORIENTED_EDGE('',*,*,#1809,.F.);
#2393=ORIENTED_EDGE('',*,*,#1826,.T.);
#2394=ORIENTED_EDGE('',*,*,#1813,.F.);
#2395=ORIENTED_EDGE('',*,*,#1827,.T.);
#2396=ORIENTED_EDGE('',*,*,#1819,.F.);
#2397=ORIENTED_EDGE('',*,*,#1828,.T.);
#2398=ORIENTED_EDGE('',*,*,#1779,.F.);
#2399=ORIENTED_EDGE('',*,*,#1811,.T.);
#2400=ORIENTED_EDGE('',*,*,#1829,.T.);
#2401=ORIENTED_EDGE('',*,*,#1821,.T.);
#2402=ORIENTED_EDGE('',*,*,#1830,.T.);
#2403=ORIENTED_EDGE('',*,*,#1817,.T.);
#2404=ORIENTED_EDGE('',*,*,#1831,.T.);
#2405=ORIENTED_EDGE('',*,*,#1815,.T.);
#2406=ORIENTED_EDGE('',*,*,#1832,.T.);
#2407=ORIENTED_EDGE('',*,*,#1776,.F.);
#2408=ORIENTED_EDGE('',*,*,#1825,.F.);
#2409=ORIENTED_EDGE('',*,*,#1822,.F.);
#2410=ORIENTED_EDGE('',*,*,#1829,.F.);
#2411=ORIENTED_EDGE('',*,*,#1810,.F.);
#2412=ORIENTED_EDGE('',*,*,#1828,.F.);
#2413=ORIENTED_EDGE('',*,*,#1818,.F.);
#2414=ORIENTED_EDGE('',*,*,#1830,.F.);
#2415=ORIENTED_EDGE('',*,*,#1824,.F.);
#2416=ORIENTED_EDGE('',*,*,#1826,.F.);
#2417=ORIENTED_EDGE('',*,*,#1812,.F.);
#2418=ORIENTED_EDGE('',*,*,#1832,.F.);
#2419=ORIENTED_EDGE('',*,*,#1814,.F.);
#2420=ORIENTED_EDGE('',*,*,#1827,.F.);
#2421=ORIENTED_EDGE('',*,*,#1816,.F.);
#2422=ORIENTED_EDGE('',*,*,#1831,.F.);
#2423=ORIENTED_EDGE('',*,*,#1820,.F.);
#2424=ORIENTED_EDGE('',*,*,#1801,.F.);
#2425=ORIENTED_EDGE('',*,*,#1790,.F.);
#2426=ORIENTED_EDGE('',*,*,#1805,.F.);
#2427=ORIENTED_EDGE('',*,*,#1794,.F.);
#2428=ORIENTED_EDGE('',*,*,#1804,.F.);
#2429=ORIENTED_EDGE('',*,*,#1786,.F.);
#2430=ORIENTED_EDGE('',*,*,#1806,.F.);
#2431=ORIENTED_EDGE('',*,*,#1792,.F.);
#2432=ORIENTED_EDGE('',*,*,#1802,.F.);
#2433=ORIENTED_EDGE('',*,*,#1796,.F.);
#2434=ORIENTED_EDGE('',*,*,#1808,.F.);
#2435=ORIENTED_EDGE('',*,*,#1798,.F.);
#2436=ORIENTED_EDGE('',*,*,#1803,.F.);
#2437=ORIENTED_EDGE('',*,*,#1800,.F.);
#2438=ORIENTED_EDGE('',*,*,#1807,.F.);
#2439=ORIENTED_EDGE('',*,*,#1788,.F.);
#2440=ORIENTED_EDGE('',*,*,#1833,.F.);
#2441=ORIENTED_EDGE('',*,*,#1834,.T.);
#2442=ORIENTED_EDGE('',*,*,#1835,.T.);
#2443=ORIENTED_EDGE('',*,*,#1834,.F.);
#2444=ORIENTED_EDGE('',*,*,#1836,.F.);
#2445=ORIENTED_EDGE('',*,*,#1837,.T.);
#2446=ORIENTED_EDGE('',*,*,#1838,.T.);
#2447=ORIENTED_EDGE('',*,*,#1837,.F.);
#2448=ORIENTED_EDGE('',*,*,#1833,.T.);
#2449=ORIENTED_EDGE('',*,*,#1838,.F.);
#2450=ORIENTED_EDGE('',*,*,#1835,.F.);
#2451=ORIENTED_EDGE('',*,*,#1836,.T.);
#2452=ORIENTED_EDGE('',*,*,#1839,.T.);
#2453=ORIENTED_EDGE('',*,*,#1840,.T.);
#2454=ORIENTED_EDGE('',*,*,#1841,.T.);
#2455=ORIENTED_EDGE('',*,*,#1840,.F.);
#2456=ORIENTED_EDGE('',*,*,#1842,.F.);
#2457=ORIENTED_EDGE('',*,*,#1843,.F.);
#2458=ORIENTED_EDGE('',*,*,#1844,.T.);
#2459=ORIENTED_EDGE('',*,*,#1845,.T.);
#2460=ORIENTED_EDGE('',*,*,#1846,.F.);
#2461=ORIENTED_EDGE('',*,*,#1847,.F.);
#2462=ORIENTED_EDGE('',*,*,#1848,.T.);
#2463=ORIENTED_EDGE('',*,*,#1849,.T.);
#2464=ORIENTED_EDGE('',*,*,#1850,.F.);
#2465=ORIENTED_EDGE('',*,*,#1851,.F.);
#2466=ORIENTED_EDGE('',*,*,#1852,.T.);
#2467=ORIENTED_EDGE('',*,*,#1853,.T.);
#2468=ORIENTED_EDGE('',*,*,#1854,.T.);
#2469=ORIENTED_EDGE('',*,*,#1855,.T.);
#2470=ORIENTED_EDGE('',*,*,#1856,.F.);
#2471=ORIENTED_EDGE('',*,*,#1857,.F.);
#2472=ORIENTED_EDGE('',*,*,#1858,.F.);
#2473=ORIENTED_EDGE('',*,*,#1859,.F.);
#2474=ORIENTED_EDGE('',*,*,#1842,.T.);
#2475=ORIENTED_EDGE('',*,*,#1860,.F.);
#2476=ORIENTED_EDGE('',*,*,#1861,.F.);
#2477=ORIENTED_EDGE('',*,*,#1846,.T.);
#2478=ORIENTED_EDGE('',*,*,#1862,.F.);
#2479=ORIENTED_EDGE('',*,*,#1863,.F.);
#2480=ORIENTED_EDGE('',*,*,#1850,.T.);
#2481=ORIENTED_EDGE('',*,*,#1864,.F.);
#2482=ORIENTED_EDGE('',*,*,#1865,.F.);
#2483=ORIENTED_EDGE('',*,*,#1856,.T.);
#2484=ORIENTED_EDGE('',*,*,#1841,.F.);
#2485=ORIENTED_EDGE('',*,*,#1866,.F.);
#2486=ORIENTED_EDGE('',*,*,#1867,.F.);
#2487=ORIENTED_EDGE('',*,*,#1854,.F.);
#2488=ORIENTED_EDGE('',*,*,#1868,.F.);
#2489=ORIENTED_EDGE('',*,*,#1869,.F.);
#2490=ORIENTED_EDGE('',*,*,#1852,.F.);
#2491=ORIENTED_EDGE('',*,*,#1870,.F.);
#2492=ORIENTED_EDGE('',*,*,#1871,.F.);
#2493=ORIENTED_EDGE('',*,*,#1848,.F.);
#2494=ORIENTED_EDGE('',*,*,#1872,.F.);
#2495=ORIENTED_EDGE('',*,*,#1873,.F.);
#2496=ORIENTED_EDGE('',*,*,#1844,.F.);
#2497=ORIENTED_EDGE('',*,*,#1839,.F.);
#2498=ORIENTED_EDGE('',*,*,#1869,.T.);
#2499=ORIENTED_EDGE('',*,*,#1874,.T.);
#2500=ORIENTED_EDGE('',*,*,#1864,.T.);
#2501=ORIENTED_EDGE('',*,*,#1853,.F.);
#2502=ORIENTED_EDGE('',*,*,#1868,.T.);
#2503=ORIENTED_EDGE('',*,*,#1857,.T.);
#2504=ORIENTED_EDGE('',*,*,#1865,.T.);
#2505=ORIENTED_EDGE('',*,*,#1874,.F.);
#2506=ORIENTED_EDGE('',*,*,#1871,.T.);
#2507=ORIENTED_EDGE('',*,*,#1875,.T.);
#2508=ORIENTED_EDGE('',*,*,#1862,.T.);
#2509=ORIENTED_EDGE('',*,*,#1849,.F.);
#2510=ORIENTED_EDGE('',*,*,#1870,.T.);
#2511=ORIENTED_EDGE('',*,*,#1851,.T.);
#2512=ORIENTED_EDGE('',*,*,#1863,.T.);
#2513=ORIENTED_EDGE('',*,*,#1875,.F.);
#2514=ORIENTED_EDGE('',*,*,#1873,.T.);
#2515=ORIENTED_EDGE('',*,*,#1876,.T.);
#2516=ORIENTED_EDGE('',*,*,#1860,.T.);
#2517=ORIENTED_EDGE('',*,*,#1845,.F.);
#2518=ORIENTED_EDGE('',*,*,#1872,.T.);
#2519=ORIENTED_EDGE('',*,*,#1847,.T.);
#2520=ORIENTED_EDGE('',*,*,#1861,.T.);
#2521=ORIENTED_EDGE('',*,*,#1876,.F.);
#2522=ORIENTED_EDGE('',*,*,#1867,.T.);
#2523=ORIENTED_EDGE('',*,*,#1877,.T.);
#2524=ORIENTED_EDGE('',*,*,#1858,.T.);
#2525=ORIENTED_EDGE('',*,*,#1855,.F.);
#2526=ORIENTED_EDGE('',*,*,#1866,.T.);
#2527=ORIENTED_EDGE('',*,*,#1843,.T.);
#2528=ORIENTED_EDGE('',*,*,#1859,.T.);
#2529=ORIENTED_EDGE('',*,*,#1877,.F.);
#2530=ORIENTED_EDGE('',*,*,#1878,.F.);
#2531=ORIENTED_EDGE('',*,*,#1879,.T.);
#2532=ORIENTED_EDGE('',*,*,#1880,.F.);
#2533=ORIENTED_EDGE('',*,*,#1881,.F.);
#2534=ORIENTED_EDGE('',*,*,#1882,.F.);
#2535=ORIENTED_EDGE('',*,*,#1883,.F.);
#2536=ORIENTED_EDGE('',*,*,#1884,.T.);
#2537=ORIENTED_EDGE('',*,*,#1885,.F.);
#2538=ORIENTED_EDGE('',*,*,#1886,.F.);
#2539=ORIENTED_EDGE('',*,*,#1887,.F.);
#2540=ORIENTED_EDGE('',*,*,#1888,.T.);
#2541=ORIENTED_EDGE('',*,*,#1889,.T.);
#2542=ORIENTED_EDGE('',*,*,#1890,.F.);
#2543=ORIENTED_EDGE('',*,*,#1891,.T.);
#2544=ORIENTED_EDGE('',*,*,#1892,.T.);
#2545=ORIENTED_EDGE('',*,*,#1893,.T.);
#2546=ORIENTED_EDGE('',*,*,#1894,.F.);
#2547=ORIENTED_EDGE('',*,*,#1893,.F.);
#2548=ORIENTED_EDGE('',*,*,#1895,.T.);
#2549=ORIENTED_EDGE('',*,*,#1896,.T.);
#2550=ORIENTED_EDGE('',*,*,#1897,.F.);
#2551=ORIENTED_EDGE('',*,*,#1898,.T.);
#2552=ORIENTED_EDGE('',*,*,#1899,.T.);
#2553=ORIENTED_EDGE('',*,*,#1878,.T.);
#2554=ORIENTED_EDGE('',*,*,#1900,.T.);
#2555=ORIENTED_EDGE('',*,*,#1883,.T.);
#2556=ORIENTED_EDGE('',*,*,#1881,.T.);
#2557=ORIENTED_EDGE('',*,*,#1901,.T.);
#2558=ORIENTED_EDGE('',*,*,#1902,.F.);
#2559=ORIENTED_EDGE('',*,*,#1901,.F.);
#2560=ORIENTED_EDGE('',*,*,#1880,.T.);
#2561=ORIENTED_EDGE('',*,*,#1903,.T.);
#2562=ORIENTED_EDGE('',*,*,#1904,.F.);
#2563=ORIENTED_EDGE('',*,*,#1905,.T.);
#2564=ORIENTED_EDGE('',*,*,#1885,.T.);
#2565=ORIENTED_EDGE('',*,*,#1906,.T.);
#2566=ORIENTED_EDGE('',*,*,#1886,.T.);
#2567=ORIENTED_EDGE('',*,*,#1905,.F.);
#2568=ORIENTED_EDGE('',*,*,#1907,.F.);
#2569=ORIENTED_EDGE('',*,*,#1908,.T.);
#2570=ORIENTED_EDGE('',*,*,#1909,.T.);
#2571=ORIENTED_EDGE('',*,*,#1908,.F.);
#2572=ORIENTED_EDGE('',*,*,#1910,.F.);
#2573=ORIENTED_EDGE('',*,*,#1911,.T.);
#2574=ORIENTED_EDGE('',*,*,#1912,.F.);
#2575=ORIENTED_EDGE('',*,*,#1911,.F.);
#2576=ORIENTED_EDGE('',*,*,#1913,.F.);
#2577=ORIENTED_EDGE('',*,*,#1914,.T.);
#2578=ORIENTED_EDGE('',*,*,#1910,.T.);
#2579=ORIENTED_EDGE('',*,*,#1914,.F.);
#2580=ORIENTED_EDGE('',*,*,#1915,.F.);
#2581=ORIENTED_EDGE('',*,*,#1916,.T.);
#2582=ORIENTED_EDGE('',*,*,#1917,.T.);
#2583=ORIENTED_EDGE('',*,*,#1916,.F.);
#2584=ORIENTED_EDGE('',*,*,#1918,.F.);
#2585=ORIENTED_EDGE('',*,*,#1919,.T.);
#2586=ORIENTED_EDGE('',*,*,#1920,.T.);
#2587=ORIENTED_EDGE('',*,*,#1919,.F.);
#2588=ORIENTED_EDGE('',*,*,#1921,.T.);
#2589=ORIENTED_EDGE('',*,*,#1922,.T.);
#2590=ORIENTED_EDGE('',*,*,#1923,.T.);
#2591=ORIENTED_EDGE('',*,*,#1922,.F.);
#2592=ORIENTED_EDGE('',*,*,#1923,.F.);
#2593=ORIENTED_EDGE('',*,*,#1918,.T.);
#2594=ORIENTED_EDGE('',*,*,#1920,.F.);
#2595=ORIENTED_EDGE('',*,*,#1915,.T.);
#2596=ORIENTED_EDGE('',*,*,#1917,.F.);
#2597=ORIENTED_EDGE('',*,*,#1913,.T.);
#2598=ORIENTED_EDGE('',*,*,#1912,.T.);
#2599=ORIENTED_EDGE('',*,*,#1894,.T.);
#2600=ORIENTED_EDGE('',*,*,#1909,.F.);
#2601=ORIENTED_EDGE('',*,*,#1921,.F.);
#2602=ORIENTED_EDGE('',*,*,#1907,.T.);
#2603=ORIENTED_EDGE('',*,*,#1884,.F.);
#2604=ORIENTED_EDGE('',*,*,#1900,.F.);
#2605=ORIENTED_EDGE('',*,*,#1887,.T.);
#2606=ORIENTED_EDGE('',*,*,#1906,.F.);
#2607=ORIENTED_EDGE('',*,*,#1879,.F.);
#2608=ORIENTED_EDGE('',*,*,#1899,.F.);
#2609=ORIENTED_EDGE('',*,*,#1882,.T.);
#2610=ORIENTED_EDGE('',*,*,#1903,.F.);
#2611=ORIENTED_EDGE('',*,*,#1897,.T.);
#2612=ORIENTED_EDGE('',*,*,#1924,.F.);
#2613=ORIENTED_EDGE('',*,*,#1925,.F.);
#2614=ORIENTED_EDGE('',*,*,#1898,.F.);
#2615=ORIENTED_EDGE('',*,*,#1924,.T.);
#2616=ORIENTED_EDGE('',*,*,#1896,.F.);
#2617=ORIENTED_EDGE('',*,*,#1904,.T.);
#2618=ORIENTED_EDGE('',*,*,#1926,.F.);
#2619=ORIENTED_EDGE('',*,*,#1888,.F.);
#2620=ORIENTED_EDGE('',*,*,#1925,.T.);
#2621=ORIENTED_EDGE('',*,*,#1895,.F.);
#2622=ORIENTED_EDGE('',*,*,#1892,.F.);
#2623=ORIENTED_EDGE('',*,*,#1926,.T.);
#2624=ORIENTED_EDGE('',*,*,#1891,.F.);
#2625=ORIENTED_EDGE('',*,*,#1927,.F.);
#2626=ORIENTED_EDGE('',*,*,#1889,.F.);
#2627=ORIENTED_EDGE('',*,*,#1902,.T.);
#2628=ORIENTED_EDGE('',*,*,#1890,.T.);
#2629=ORIENTED_EDGE('',*,*,#1927,.T.);
#2630=ORIENTED_EDGE('',*,*,#1928,.F.);
#2631=ORIENTED_EDGE('',*,*,#1929,.F.);
#2632=ORIENTED_EDGE('',*,*,#1930,.F.);
#2633=ORIENTED_EDGE('',*,*,#1931,.F.);
#2634=ORIENTED_EDGE('',*,*,#1932,.T.);
#2635=ORIENTED_EDGE('',*,*,#1933,.T.);
#2636=ORIENTED_EDGE('',*,*,#1934,.T.);
#2637=ORIENTED_EDGE('',*,*,#1935,.F.);
#2638=ORIENTED_EDGE('',*,*,#1936,.F.);
#2639=ORIENTED_EDGE('',*,*,#1937,.T.);
#2640=ORIENTED_EDGE('',*,*,#1938,.T.);
#2641=ORIENTED_EDGE('',*,*,#1931,.T.);
#2642=ORIENTED_EDGE('',*,*,#1939,.F.);
#2643=ORIENTED_EDGE('',*,*,#1940,.T.);
#2644=ORIENTED_EDGE('',*,*,#1936,.T.);
#2645=ORIENTED_EDGE('',*,*,#1930,.T.);
#2646=ORIENTED_EDGE('',*,*,#1941,.F.);
#2647=ORIENTED_EDGE('',*,*,#1942,.F.);
#2648=ORIENTED_EDGE('',*,*,#1943,.F.);
#2649=ORIENTED_EDGE('',*,*,#1934,.F.);
#2650=ORIENTED_EDGE('',*,*,#1938,.F.);
#2651=ORIENTED_EDGE('',*,*,#1944,.T.);
#2652=ORIENTED_EDGE('',*,*,#1945,.F.);
#2653=ORIENTED_EDGE('',*,*,#1932,.F.);
#2654=ORIENTED_EDGE('',*,*,#1946,.F.);
#2655=ORIENTED_EDGE('',*,*,#1947,.F.);
#2656=ORIENTED_EDGE('',*,*,#1948,.F.);
#2657=ORIENTED_EDGE('',*,*,#1928,.T.);
#2658=ORIENTED_EDGE('',*,*,#1947,.T.);
#2659=ORIENTED_EDGE('',*,*,#1949,.T.);
#2660=ORIENTED_EDGE('',*,*,#1942,.T.);
#2661=ORIENTED_EDGE('',*,*,#1950,.F.);
#2662=ORIENTED_EDGE('',*,*,#1946,.T.);
#2663=ORIENTED_EDGE('',*,*,#1935,.T.);
#2664=ORIENTED_EDGE('',*,*,#1943,.T.);
#2665=ORIENTED_EDGE('',*,*,#1949,.F.);
#2666=ORIENTED_EDGE('',*,*,#1945,.T.);
#2667=ORIENTED_EDGE('',*,*,#1951,.T.);
#2668=ORIENTED_EDGE('',*,*,#1939,.T.);
#2669=ORIENTED_EDGE('',*,*,#1933,.F.);
#2670=ORIENTED_EDGE('',*,*,#1941,.T.);
#2671=ORIENTED_EDGE('',*,*,#1929,.T.);
#2672=ORIENTED_EDGE('',*,*,#1948,.T.);
#2673=ORIENTED_EDGE('',*,*,#1950,.T.);
#2674=ORIENTED_EDGE('',*,*,#1944,.F.);
#2675=ORIENTED_EDGE('',*,*,#1937,.F.);
#2676=ORIENTED_EDGE('',*,*,#1940,.F.);
#2677=ORIENTED_EDGE('',*,*,#1951,.F.);
#2678=ORIENTED_EDGE('',*,*,#1952,.F.);
#2679=ORIENTED_EDGE('',*,*,#1953,.T.);
#2680=ORIENTED_EDGE('',*,*,#1954,.F.);
#2681=ORIENTED_EDGE('',*,*,#1953,.F.);
#2682=ORIENTED_EDGE('',*,*,#1955,.F.);
#2683=ORIENTED_EDGE('',*,*,#1956,.T.);
#2684=ORIENTED_EDGE('',*,*,#1952,.T.);
#2685=ORIENTED_EDGE('',*,*,#1956,.F.);
#2686=ORIENTED_EDGE('',*,*,#1957,.F.);
#2687=ORIENTED_EDGE('',*,*,#1958,.T.);
#2688=ORIENTED_EDGE('',*,*,#1959,.F.);
#2689=ORIENTED_EDGE('',*,*,#1960,.F.);
#2690=ORIENTED_EDGE('',*,*,#1961,.T.);
#2691=ORIENTED_EDGE('',*,*,#1962,.F.);
#2692=ORIENTED_EDGE('',*,*,#1963,.F.);
#2693=ORIENTED_EDGE('',*,*,#1964,.F.);
#2694=ORIENTED_EDGE('',*,*,#1965,.F.);
#2695=ORIENTED_EDGE('',*,*,#1966,.T.);
#2696=ORIENTED_EDGE('',*,*,#1967,.F.);
#2697=ORIENTED_EDGE('',*,*,#1968,.F.);
#2698=ORIENTED_EDGE('',*,*,#1969,.F.);
#2699=ORIENTED_EDGE('',*,*,#1970,.F.);
#2700=ORIENTED_EDGE('',*,*,#1970,.T.);
#2701=ORIENTED_EDGE('',*,*,#1971,.T.);
#2702=ORIENTED_EDGE('',*,*,#1972,.T.);
#2703=ORIENTED_EDGE('',*,*,#1969,.T.);
#2704=ORIENTED_EDGE('',*,*,#1972,.F.);
#2705=ORIENTED_EDGE('',*,*,#1973,.T.);
#2706=ORIENTED_EDGE('',*,*,#1974,.T.);
#2707=ORIENTED_EDGE('',*,*,#1975,.T.);
#2708=ORIENTED_EDGE('',*,*,#1976,.T.);
#2709=ORIENTED_EDGE('',*,*,#1977,.T.);
#2710=ORIENTED_EDGE('',*,*,#1978,.T.);
#2711=ORIENTED_EDGE('',*,*,#1979,.T.);
#2712=ORIENTED_EDGE('',*,*,#1980,.T.);
#2713=ORIENTED_EDGE('',*,*,#1981,.T.);
#2714=ORIENTED_EDGE('',*,*,#1982,.T.);
#2715=ORIENTED_EDGE('',*,*,#1983,.T.);
#2716=ORIENTED_EDGE('',*,*,#1984,.T.);
#2717=ORIENTED_EDGE('',*,*,#1985,.T.);
#2718=ORIENTED_EDGE('',*,*,#1986,.T.);
#2719=ORIENTED_EDGE('',*,*,#1987,.T.);
#2720=ORIENTED_EDGE('',*,*,#1988,.T.);
#2721=ORIENTED_EDGE('',*,*,#1989,.T.);
#2722=ORIENTED_EDGE('',*,*,#1990,.T.);
#2723=ORIENTED_EDGE('',*,*,#1991,.T.);
#2724=ORIENTED_EDGE('',*,*,#1992,.T.);
#2725=ORIENTED_EDGE('',*,*,#1993,.T.);
#2726=ORIENTED_EDGE('',*,*,#1994,.T.);
#2727=ORIENTED_EDGE('',*,*,#1995,.T.);
#2728=ORIENTED_EDGE('',*,*,#1996,.T.);
#2729=ORIENTED_EDGE('',*,*,#1997,.T.);
#2730=ORIENTED_EDGE('',*,*,#1998,.T.);
#2731=ORIENTED_EDGE('',*,*,#1999,.T.);
#2732=ORIENTED_EDGE('',*,*,#2000,.T.);
#2733=ORIENTED_EDGE('',*,*,#2001,.T.);
#2734=ORIENTED_EDGE('',*,*,#2002,.T.);
#2735=ORIENTED_EDGE('',*,*,#2003,.T.);
#2736=ORIENTED_EDGE('',*,*,#2004,.T.);
#2737=ORIENTED_EDGE('',*,*,#2005,.T.);
#2738=ORIENTED_EDGE('',*,*,#2006,.T.);
#2739=ORIENTED_EDGE('',*,*,#2007,.T.);
#2740=ORIENTED_EDGE('',*,*,#2008,.T.);
#2741=ORIENTED_EDGE('',*,*,#2009,.T.);
#2742=ORIENTED_EDGE('',*,*,#2010,.T.);
#2743=ORIENTED_EDGE('',*,*,#2011,.T.);
#2744=ORIENTED_EDGE('',*,*,#2012,.T.);
#2745=ORIENTED_EDGE('',*,*,#2013,.T.);
#2746=ORIENTED_EDGE('',*,*,#2014,.T.);
#2747=ORIENTED_EDGE('',*,*,#2015,.T.);
#2748=ORIENTED_EDGE('',*,*,#2016,.T.);
#2749=ORIENTED_EDGE('',*,*,#2017,.T.);
#2750=ORIENTED_EDGE('',*,*,#2018,.T.);
#2751=ORIENTED_EDGE('',*,*,#2019,.T.);
#2752=ORIENTED_EDGE('',*,*,#2020,.T.);
#2753=ORIENTED_EDGE('',*,*,#2021,.T.);
#2754=ORIENTED_EDGE('',*,*,#2022,.T.);
#2755=ORIENTED_EDGE('',*,*,#2023,.T.);
#2756=ORIENTED_EDGE('',*,*,#1962,.T.);
#2757=ORIENTED_EDGE('',*,*,#2024,.T.);
#2758=ORIENTED_EDGE('',*,*,#2025,.T.);
#2759=ORIENTED_EDGE('',*,*,#2026,.T.);
#2760=ORIENTED_EDGE('',*,*,#1964,.T.);
#2761=ORIENTED_EDGE('',*,*,#2027,.T.);
#2762=ORIENTED_EDGE('',*,*,#2028,.T.);
#2763=ORIENTED_EDGE('',*,*,#2029,.T.);
#2764=ORIENTED_EDGE('',*,*,#2030,.T.);
#2765=ORIENTED_EDGE('',*,*,#2031,.F.);
#2766=ORIENTED_EDGE('',*,*,#2032,.T.);
#2767=ORIENTED_EDGE('',*,*,#2033,.T.);
#2768=ORIENTED_EDGE('',*,*,#2034,.T.);
#2769=ORIENTED_EDGE('',*,*,#1967,.T.);
#2770=ORIENTED_EDGE('',*,*,#2035,.T.);
#2771=ORIENTED_EDGE('',*,*,#2036,.T.);
#2772=ORIENTED_EDGE('',*,*,#2037,.T.);
#2773=ORIENTED_EDGE('',*,*,#2038,.T.);
#2774=ORIENTED_EDGE('',*,*,#2039,.T.);
#2775=ORIENTED_EDGE('',*,*,#2040,.T.);
#2776=ORIENTED_EDGE('',*,*,#2041,.T.);
#2777=ORIENTED_EDGE('',*,*,#1971,.F.);
#2778=ORIENTED_EDGE('',*,*,#2042,.T.);
#2779=ORIENTED_EDGE('',*,*,#2043,.T.);
#2780=ORIENTED_EDGE('',*,*,#2044,.T.);
#2781=ORIENTED_EDGE('',*,*,#1957,.T.);
#2782=ORIENTED_EDGE('',*,*,#2045,.T.);
#2783=ORIENTED_EDGE('',*,*,#2046,.T.);
#2784=ORIENTED_EDGE('',*,*,#2047,.T.);
#2785=ORIENTED_EDGE('',*,*,#2048,.T.);
#2786=ORIENTED_EDGE('',*,*,#2049,.T.);
#2787=ORIENTED_EDGE('',*,*,#2050,.T.);
#2788=ORIENTED_EDGE('',*,*,#2051,.T.);
#2789=ORIENTED_EDGE('',*,*,#2052,.T.);
#2790=ORIENTED_EDGE('',*,*,#1954,.T.);
#2791=ORIENTED_EDGE('',*,*,#1965,.T.);
#2792=ORIENTED_EDGE('',*,*,#2053,.T.);
#2793=ORIENTED_EDGE('',*,*,#2054,.T.);
#2794=ORIENTED_EDGE('',*,*,#2055,.T.);
#2795=ORIENTED_EDGE('',*,*,#2056,.T.);
#2796=ORIENTED_EDGE('',*,*,#2057,.T.);
#2797=ORIENTED_EDGE('',*,*,#2058,.T.);
#2798=ORIENTED_EDGE('',*,*,#2059,.T.);
#2799=ORIENTED_EDGE('',*,*,#2060,.T.);
#2800=ORIENTED_EDGE('',*,*,#2061,.T.);
#2801=ORIENTED_EDGE('',*,*,#2062,.T.);
#2802=ORIENTED_EDGE('',*,*,#2031,.T.);
#2803=ORIENTED_EDGE('',*,*,#2063,.T.);
#2804=ORIENTED_EDGE('',*,*,#2064,.T.);
#2805=ORIENTED_EDGE('',*,*,#2065,.T.);
#2806=ORIENTED_EDGE('',*,*,#2066,.T.);
#2807=ORIENTED_EDGE('',*,*,#1959,.T.);
#2808=ORIENTED_EDGE('',*,*,#2067,.T.);
#2809=ORIENTED_EDGE('',*,*,#2068,.T.);
#2810=ORIENTED_EDGE('',*,*,#2069,.T.);
#2811=ORIENTED_EDGE('',*,*,#2070,.T.);
#2812=ORIENTED_EDGE('',*,*,#2071,.T.);
#2813=ORIENTED_EDGE('',*,*,#2072,.T.);
#2814=ORIENTED_EDGE('',*,*,#2073,.T.);
#2815=ORIENTED_EDGE('',*,*,#2074,.T.);
#2816=ORIENTED_EDGE('',*,*,#2075,.T.);
#2817=ORIENTED_EDGE('',*,*,#2076,.F.);
#2818=ORIENTED_EDGE('',*,*,#2077,.F.);
#2819=ORIENTED_EDGE('',*,*,#2078,.F.);
#2820=ORIENTED_EDGE('',*,*,#2077,.T.);
#2821=ORIENTED_EDGE('',*,*,#2010,.F.);
#2822=ORIENTED_EDGE('',*,*,#2079,.F.);
#2823=ORIENTED_EDGE('',*,*,#2037,.F.);
#2824=ORIENTED_EDGE('',*,*,#2078,.T.);
#2825=ORIENTED_EDGE('',*,*,#2036,.F.);
#2826=ORIENTED_EDGE('',*,*,#2080,.F.);
#2827=ORIENTED_EDGE('',*,*,#2057,.F.);
#2828=ORIENTED_EDGE('',*,*,#2081,.F.);
#2829=ORIENTED_EDGE('',*,*,#2055,.F.);
#2830=ORIENTED_EDGE('',*,*,#2082,.F.);
#2831=ORIENTED_EDGE('',*,*,#2005,.F.);
#2832=ORIENTED_EDGE('',*,*,#2076,.T.);
#2833=ORIENTED_EDGE('',*,*,#2056,.F.);
#2834=ORIENTED_EDGE('',*,*,#2083,.F.);
#2835=ORIENTED_EDGE('',*,*,#2011,.F.);
#2836=ORIENTED_EDGE('',*,*,#2084,.F.);
#2837=ORIENTED_EDGE('',*,*,#2009,.F.);
#2838=ORIENTED_EDGE('',*,*,#2085,.F.);
#2839=ORIENTED_EDGE('',*,*,#1983,.F.);
#2840=ORIENTED_EDGE('',*,*,#2079,.T.);
#2841=ORIENTED_EDGE('',*,*,#2084,.T.);
#2842=ORIENTED_EDGE('',*,*,#2086,.F.);
#2843=ORIENTED_EDGE('',*,*,#2082,.T.);
#2844=ORIENTED_EDGE('',*,*,#2080,.T.);
#2845=ORIENTED_EDGE('',*,*,#2087,.F.);
#2846=ORIENTED_EDGE('',*,*,#2083,.T.);
#2847=ORIENTED_EDGE('',*,*,#2081,.T.);
#2848=ORIENTED_EDGE('',*,*,#2088,.F.);
#2849=ORIENTED_EDGE('',*,*,#2089,.F.);
#2850=ORIENTED_EDGE('',*,*,#2090,.F.);
#2851=ORIENTED_EDGE('',*,*,#2085,.T.);
#2852=ORIENTED_EDGE('',*,*,#2090,.T.);
#2853=ORIENTED_EDGE('',*,*,#2019,.F.);
#2854=ORIENTED_EDGE('',*,*,#2091,.F.);
#2855=ORIENTED_EDGE('',*,*,#1984,.F.);
#2856=ORIENTED_EDGE('',*,*,#2086,.T.);
#2857=ORIENTED_EDGE('',*,*,#1982,.F.);
#2858=ORIENTED_EDGE('',*,*,#2092,.F.);
#2859=ORIENTED_EDGE('',*,*,#2038,.F.);
#2860=ORIENTED_EDGE('',*,*,#2087,.T.);
#2861=ORIENTED_EDGE('',*,*,#2035,.F.);
#2862=ORIENTED_EDGE('',*,*,#2093,.F.);
#2863=ORIENTED_EDGE('',*,*,#2006,.F.);
#2864=ORIENTED_EDGE('',*,*,#2088,.T.);
#2865=ORIENTED_EDGE('',*,*,#2004,.F.);
#2866=ORIENTED_EDGE('',*,*,#2094,.F.);
#2867=ORIENTED_EDGE('',*,*,#2012,.F.);
#2868=ORIENTED_EDGE('',*,*,#2095,.F.);
#2869=ORIENTED_EDGE('',*,*,#2013,.F.);
#2870=ORIENTED_EDGE('',*,*,#2096,.F.);
#2871=ORIENTED_EDGE('',*,*,#2068,.F.);
#2872=ORIENTED_EDGE('',*,*,#2097,.F.);
#2873=ORIENTED_EDGE('',*,*,#2014,.F.);
#2874=ORIENTED_EDGE('',*,*,#2098,.F.);
#2875=ORIENTED_EDGE('',*,*,#2042,.F.);
#2876=ORIENTED_EDGE('',*,*,#2099,.F.);
#2877=ORIENTED_EDGE('',*,*,#2015,.F.);
#2878=ORIENTED_EDGE('',*,*,#2100,.F.);
#2879=ORIENTED_EDGE('',*,*,#1978,.F.);
#2880=ORIENTED_EDGE('',*,*,#2089,.T.);
#2881=ORIENTED_EDGE('',*,*,#2016,.F.);
#2882=ORIENTED_EDGE('',*,*,#2101,.F.);
#2883=ORIENTED_EDGE('',*,*,#2020,.F.);
#2884=ORIENTED_EDGE('',*,*,#2092,.T.);
#2885=ORIENTED_EDGE('',*,*,#2091,.T.);
#2886=ORIENTED_EDGE('',*,*,#2102,.F.);
#2887=ORIENTED_EDGE('',*,*,#2103,.F.);
#2888=ORIENTED_EDGE('',*,*,#2093,.T.);
#2889=ORIENTED_EDGE('',*,*,#1966,.F.);
#2890=ORIENTED_EDGE('',*,*,#2096,.T.);
#2891=ORIENTED_EDGE('',*,*,#2094,.T.);
#2892=ORIENTED_EDGE('',*,*,#2104,.F.);
#2893=ORIENTED_EDGE('',*,*,#2098,.T.);
#2894=ORIENTED_EDGE('',*,*,#2095,.T.);
#2895=ORIENTED_EDGE('',*,*,#2105,.F.);
#2896=ORIENTED_EDGE('',*,*,#2100,.T.);
#2897=ORIENTED_EDGE('',*,*,#2097,.T.);
#2898=ORIENTED_EDGE('',*,*,#2106,.F.);
#2899=ORIENTED_EDGE('',*,*,#2101,.T.);
#2900=ORIENTED_EDGE('',*,*,#2099,.T.);
#2901=ORIENTED_EDGE('',*,*,#2107,.F.);
#2902=ORIENTED_EDGE('',*,*,#2102,.T.);
#2903=ORIENTED_EDGE('',*,*,#2018,.F.);
#2904=ORIENTED_EDGE('',*,*,#2108,.F.);
#2905=ORIENTED_EDGE('',*,*,#2039,.F.);
#2906=ORIENTED_EDGE('',*,*,#2109,.F.);
#2907=ORIENTED_EDGE('',*,*,#2053,.F.);
#2908=ORIENTED_EDGE('',*,*,#2110,.F.);
#2909=ORIENTED_EDGE('',*,*,#1997,.F.);
#2910=ORIENTED_EDGE('',*,*,#2103,.T.);
#2911=ORIENTED_EDGE('',*,*,#2054,.F.);
#2912=ORIENTED_EDGE('',*,*,#2111,.F.);
#2913=ORIENTED_EDGE('',*,*,#2007,.F.);
#2914=ORIENTED_EDGE('',*,*,#2104,.T.);
#2915=ORIENTED_EDGE('',*,*,#2003,.F.);
#2916=ORIENTED_EDGE('',*,*,#2112,.F.);
#2917=ORIENTED_EDGE('',*,*,#2069,.F.);
#2918=ORIENTED_EDGE('',*,*,#2105,.T.);
#2919=ORIENTED_EDGE('',*,*,#2067,.F.);
#2920=ORIENTED_EDGE('',*,*,#2113,.F.);
#2921=ORIENTED_EDGE('',*,*,#2043,.F.);
#2922=ORIENTED_EDGE('',*,*,#2106,.T.);
#2923=ORIENTED_EDGE('',*,*,#2052,.F.);
#2924=ORIENTED_EDGE('',*,*,#2114,.F.);
#2925=ORIENTED_EDGE('',*,*,#1976,.F.);
#2926=ORIENTED_EDGE('',*,*,#2107,.T.);
#2927=ORIENTED_EDGE('',*,*,#1977,.F.);
#2928=ORIENTED_EDGE('',*,*,#2115,.F.);
#2929=ORIENTED_EDGE('',*,*,#2021,.F.);
#2930=ORIENTED_EDGE('',*,*,#2116,.F.);
#2931=ORIENTED_EDGE('',*,*,#2017,.F.);
#2932=ORIENTED_EDGE('',*,*,#2117,.F.);
#2933=ORIENTED_EDGE('',*,*,#2058,.F.);
#2934=ORIENTED_EDGE('',*,*,#2108,.T.);
#2935=ORIENTED_EDGE('',*,*,#2116,.T.);
#2936=ORIENTED_EDGE('',*,*,#2118,.F.);
#2937=ORIENTED_EDGE('',*,*,#2110,.T.);
#2938=ORIENTED_EDGE('',*,*,#1968,.T.);
#2939=ORIENTED_EDGE('',*,*,#2119,.F.);
#2940=ORIENTED_EDGE('',*,*,#2111,.T.);
#2941=ORIENTED_EDGE('',*,*,#2109,.T.);
#2942=ORIENTED_EDGE('',*,*,#2120,.F.);
#2943=ORIENTED_EDGE('',*,*,#2113,.T.);
#2944=ORIENTED_EDGE('',*,*,#2112,.T.);
#2945=ORIENTED_EDGE('',*,*,#2121,.F.);
#2946=ORIENTED_EDGE('',*,*,#2115,.T.);
#2947=ORIENTED_EDGE('',*,*,#2114,.T.);
#2948=ORIENTED_EDGE('',*,*,#2122,.F.);
#2949=ORIENTED_EDGE('',*,*,#1961,.F.);
#2950=ORIENTED_EDGE('',*,*,#2123,.F.);
#2951=ORIENTED_EDGE('',*,*,#2117,.T.);
#2952=ORIENTED_EDGE('',*,*,#2123,.T.);
#2953=ORIENTED_EDGE('',*,*,#2026,.F.);
#2954=ORIENTED_EDGE('',*,*,#2124,.F.);
#2955=ORIENTED_EDGE('',*,*,#2059,.F.);
#2956=ORIENTED_EDGE('',*,*,#2118,.T.);
#2957=ORIENTED_EDGE('',*,*,#2060,.F.);
#2958=ORIENTED_EDGE('',*,*,#2125,.F.);
#2959=ORIENTED_EDGE('',*,*,#2040,.F.);
#2960=ORIENTED_EDGE('',*,*,#2126,.F.);
#2961=ORIENTED_EDGE('',*,*,#2033,.F.);
#2962=ORIENTED_EDGE('',*,*,#2127,.F.);
#2963=ORIENTED_EDGE('',*,*,#1979,.F.);
#2964=ORIENTED_EDGE('',*,*,#2119,.T.);
#2965=ORIENTED_EDGE('',*,*,#2034,.F.);
#2966=ORIENTED_EDGE('',*,*,#2128,.F.);
#2967=ORIENTED_EDGE('',*,*,#1998,.F.);
#2968=ORIENTED_EDGE('',*,*,#2120,.T.);
#2969=ORIENTED_EDGE('',*,*,#1996,.F.);
#2970=ORIENTED_EDGE('',*,*,#2129,.F.);
#2971=ORIENTED_EDGE('',*,*,#2008,.F.);
#2972=ORIENTED_EDGE('',*,*,#2130,.F.);
#2973=ORIENTED_EDGE('',*,*,#2001,.F.);
#2974=ORIENTED_EDGE('',*,*,#2131,.F.);
#2975=ORIENTED_EDGE('',*,*,#2065,.F.);
#2976=ORIENTED_EDGE('',*,*,#2121,.T.);
#2977=ORIENTED_EDGE('',*,*,#2002,.F.);
#2978=ORIENTED_EDGE('',*,*,#2132,.F.);
#2979=ORIENTED_EDGE('',*,*,#2044,.F.);
#2980=ORIENTED_EDGE('',*,*,#2122,.T.);
#2981=ORIENTED_EDGE('',*,*,#2051,.F.);
#2982=ORIENTED_EDGE('',*,*,#2133,.F.);
#2983=ORIENTED_EDGE('',*,*,#2022,.F.);
#2984=ORIENTED_EDGE('',*,*,#2134,.F.);
#2985=ORIENTED_EDGE('',*,*,#2023,.F.);
#2986=ORIENTED_EDGE('',*,*,#2135,.F.);
#2987=ORIENTED_EDGE('',*,*,#2072,.F.);
#2988=ORIENTED_EDGE('',*,*,#2125,.T.);
#2989=ORIENTED_EDGE('',*,*,#2124,.T.);
#2990=ORIENTED_EDGE('',*,*,#2136,.F.);
#2991=ORIENTED_EDGE('',*,*,#2137,.F.);
#2992=ORIENTED_EDGE('',*,*,#2127,.T.);
#2993=ORIENTED_EDGE('',*,*,#2138,.F.);
#2994=ORIENTED_EDGE('',*,*,#2128,.T.);
#2995=ORIENTED_EDGE('',*,*,#2126,.T.);
#2996=ORIENTED_EDGE('',*,*,#2139,.F.);
#2997=ORIENTED_EDGE('',*,*,#2131,.T.);
#2998=ORIENTED_EDGE('',*,*,#2129,.T.);
#2999=ORIENTED_EDGE('',*,*,#2140,.F.);
#3000=ORIENTED_EDGE('',*,*,#2132,.T.);
#3001=ORIENTED_EDGE('',*,*,#2130,.T.);
#3002=ORIENTED_EDGE('',*,*,#1958,.F.);
#3003=ORIENTED_EDGE('',*,*,#2135,.T.);
#3004=ORIENTED_EDGE('',*,*,#2133,.T.);
#3005=ORIENTED_EDGE('',*,*,#2141,.F.);
#3006=ORIENTED_EDGE('',*,*,#1963,.T.);
#3007=ORIENTED_EDGE('',*,*,#2134,.T.);
#3008=ORIENTED_EDGE('',*,*,#2142,.F.);
#3009=ORIENTED_EDGE('',*,*,#2136,.T.);
#3010=ORIENTED_EDGE('',*,*,#2025,.F.);
#3011=ORIENTED_EDGE('',*,*,#2143,.F.);
#3012=ORIENTED_EDGE('',*,*,#2063,.F.);
#3013=ORIENTED_EDGE('',*,*,#2041,.F.);
#3014=ORIENTED_EDGE('',*,*,#2032,.F.);
#3015=ORIENTED_EDGE('',*,*,#2062,.F.);
#3016=ORIENTED_EDGE('',*,*,#2144,.F.);
#3017=ORIENTED_EDGE('',*,*,#1991,.F.);
#3018=ORIENTED_EDGE('',*,*,#2138,.T.);
#3019=ORIENTED_EDGE('',*,*,#2137,.T.);
#3020=ORIENTED_EDGE('',*,*,#1990,.F.);
#3021=ORIENTED_EDGE('',*,*,#2145,.F.);
#3022=ORIENTED_EDGE('',*,*,#1980,.F.);
#3023=ORIENTED_EDGE('',*,*,#2139,.T.);
#3024=ORIENTED_EDGE('',*,*,#1981,.F.);
#3025=ORIENTED_EDGE('',*,*,#2146,.F.);
#3026=ORIENTED_EDGE('',*,*,#1999,.F.);
#3027=ORIENTED_EDGE('',*,*,#2140,.T.);
#3028=ORIENTED_EDGE('',*,*,#1995,.F.);
#3029=ORIENTED_EDGE('',*,*,#2147,.F.);
#3030=ORIENTED_EDGE('',*,*,#2066,.F.);
#3031=ORIENTED_EDGE('',*,*,#2141,.T.);
#3032=ORIENTED_EDGE('',*,*,#2050,.F.);
#3033=ORIENTED_EDGE('',*,*,#2148,.F.);
#3034=ORIENTED_EDGE('',*,*,#2070,.F.);
#3035=ORIENTED_EDGE('',*,*,#2142,.T.);
#3036=ORIENTED_EDGE('',*,*,#2071,.F.);
#3037=ORIENTED_EDGE('',*,*,#2149,.F.);
#3038=ORIENTED_EDGE('',*,*,#2027,.F.);
#3039=ORIENTED_EDGE('',*,*,#2143,.T.);
#3040=ORIENTED_EDGE('',*,*,#2024,.F.);
#3041=ORIENTED_EDGE('',*,*,#2150,.F.);
#3042=ORIENTED_EDGE('',*,*,#2064,.F.);
#3043=ORIENTED_EDGE('',*,*,#2144,.T.);
#3044=ORIENTED_EDGE('',*,*,#2061,.F.);
#3045=ORIENTED_EDGE('',*,*,#2151,.F.);
#3046=ORIENTED_EDGE('',*,*,#1992,.F.);
#3047=ORIENTED_EDGE('',*,*,#2146,.T.);
#3048=ORIENTED_EDGE('',*,*,#2145,.T.);
#3049=ORIENTED_EDGE('',*,*,#2152,.F.);
#3050=ORIENTED_EDGE('',*,*,#1960,.T.);
#3051=ORIENTED_EDGE('',*,*,#2147,.T.);
#3052=ORIENTED_EDGE('',*,*,#2153,.F.);
#3053=ORIENTED_EDGE('',*,*,#2149,.T.);
#3054=ORIENTED_EDGE('',*,*,#2148,.T.);
#3055=ORIENTED_EDGE('',*,*,#2154,.F.);
#3056=ORIENTED_EDGE('',*,*,#2151,.T.);
#3057=ORIENTED_EDGE('',*,*,#2150,.T.);
#3058=ORIENTED_EDGE('',*,*,#2155,.F.);
#3059=ORIENTED_EDGE('',*,*,#2152,.T.);
#3060=ORIENTED_EDGE('',*,*,#1989,.F.);
#3061=ORIENTED_EDGE('',*,*,#2156,.F.);
#3062=ORIENTED_EDGE('',*,*,#2000,.F.);
#3063=ORIENTED_EDGE('',*,*,#2157,.F.);
#3064=ORIENTED_EDGE('',*,*,#1993,.F.);
#3065=ORIENTED_EDGE('',*,*,#2158,.F.);
#3066=ORIENTED_EDGE('',*,*,#1974,.F.);
#3067=ORIENTED_EDGE('',*,*,#2153,.T.);
#3068=ORIENTED_EDGE('',*,*,#1994,.F.);
#3069=ORIENTED_EDGE('',*,*,#2159,.F.);
#3070=ORIENTED_EDGE('',*,*,#2045,.F.);
#3071=ORIENTED_EDGE('',*,*,#2154,.T.);
#3072=ORIENTED_EDGE('',*,*,#2049,.F.);
#3073=ORIENTED_EDGE('',*,*,#2160,.F.);
#3074=ORIENTED_EDGE('',*,*,#2028,.F.);
#3075=ORIENTED_EDGE('',*,*,#2161,.F.);
#3076=ORIENTED_EDGE('',*,*,#2029,.F.);
#3077=ORIENTED_EDGE('',*,*,#2162,.F.);
#3078=ORIENTED_EDGE('',*,*,#2075,.F.);
#3079=ORIENTED_EDGE('',*,*,#2155,.T.);
#3080=ORIENTED_EDGE('',*,*,#2030,.F.);
#3081=ORIENTED_EDGE('',*,*,#2163,.F.);
#3082=ORIENTED_EDGE('',*,*,#1985,.F.);
#3083=ORIENTED_EDGE('',*,*,#2158,.T.);
#3084=ORIENTED_EDGE('',*,*,#2156,.T.);
#3085=ORIENTED_EDGE('',*,*,#2164,.F.);
#3086=ORIENTED_EDGE('',*,*,#2159,.T.);
#3087=ORIENTED_EDGE('',*,*,#2157,.T.);
#3088=ORIENTED_EDGE('',*,*,#2165,.F.);
#3089=ORIENTED_EDGE('',*,*,#2162,.T.);
#3090=ORIENTED_EDGE('',*,*,#2160,.T.);
#3091=ORIENTED_EDGE('',*,*,#2166,.F.);
#3092=ORIENTED_EDGE('',*,*,#2163,.T.);
#3093=ORIENTED_EDGE('',*,*,#2161,.T.);
#3094=ORIENTED_EDGE('',*,*,#2167,.F.);
#3095=ORIENTED_EDGE('',*,*,#2164,.T.);
#3096=ORIENTED_EDGE('',*,*,#1988,.F.);
#3097=ORIENTED_EDGE('',*,*,#2168,.F.);
#3098=ORIENTED_EDGE('',*,*,#1975,.F.);
#3099=ORIENTED_EDGE('',*,*,#2165,.T.);
#3100=ORIENTED_EDGE('',*,*,#1973,.F.);
#3101=ORIENTED_EDGE('',*,*,#2169,.F.);
#3102=ORIENTED_EDGE('',*,*,#2046,.F.);
#3103=ORIENTED_EDGE('',*,*,#2166,.T.);
#3104=ORIENTED_EDGE('',*,*,#2048,.F.);
#3105=ORIENTED_EDGE('',*,*,#2170,.F.);
#3106=ORIENTED_EDGE('',*,*,#2073,.F.);
#3107=ORIENTED_EDGE('',*,*,#2167,.T.);
#3108=ORIENTED_EDGE('',*,*,#2074,.F.);
#3109=ORIENTED_EDGE('',*,*,#2171,.F.);
#3110=ORIENTED_EDGE('',*,*,#1986,.F.);
#3111=ORIENTED_EDGE('',*,*,#2169,.T.);
#3112=ORIENTED_EDGE('',*,*,#2168,.T.);
#3113=ORIENTED_EDGE('',*,*,#2172,.F.);
#3114=ORIENTED_EDGE('',*,*,#2171,.T.);
#3115=ORIENTED_EDGE('',*,*,#2170,.T.);
#3116=ORIENTED_EDGE('',*,*,#2173,.F.);
#3117=ORIENTED_EDGE('',*,*,#2172,.T.);
#3118=ORIENTED_EDGE('',*,*,#1987,.F.);
#3119=ORIENTED_EDGE('',*,*,#2173,.T.);
#3120=ORIENTED_EDGE('',*,*,#2047,.F.);
#3121=ORIENTED_EDGE('',*,*,#1955,.T.);
#3122=ORIENTED_EDGE('',*,*,#2174,.F.);
#3123=ORIENTED_EDGE('',*,*,#2175,.T.);
#3124=ORIENTED_EDGE('',*,*,#2174,.T.);
#3125=ORIENTED_EDGE('',*,*,#2175,.F.);
#3126=ORIENTED_EDGE('',*,*,#2176,.F.);
#3127=ORIENTED_EDGE('',*,*,#2177,.T.);
#3128=ORIENTED_EDGE('',*,*,#2176,.T.);
#3129=ORIENTED_EDGE('',*,*,#2177,.F.);
#3130=ORIENTED_EDGE('',*,*,#2178,.F.);
#3131=ORIENTED_EDGE('',*,*,#2179,.T.);
#3132=ORIENTED_EDGE('',*,*,#2178,.T.);
#3133=ORIENTED_EDGE('',*,*,#2179,.F.);
#3134=ORIENTED_EDGE('',*,*,#2180,.T.);
#3135=ORIENTED_EDGE('',*,*,#2181,.T.);
#3136=ORIENTED_EDGE('',*,*,#2182,.T.);
#3137=ORIENTED_EDGE('',*,*,#2183,.T.);
#3138=ORIENTED_EDGE('',*,*,#2182,.F.);
#3139=ORIENTED_EDGE('',*,*,#2184,.T.);
#3140=ORIENTED_EDGE('',*,*,#2185,.T.);
#3141=ORIENTED_EDGE('',*,*,#2186,.F.);
#3142=ORIENTED_EDGE('',*,*,#2183,.F.);
#3143=ORIENTED_EDGE('',*,*,#2184,.F.);
#3144=ORIENTED_EDGE('',*,*,#2181,.F.);
#3145=ORIENTED_EDGE('',*,*,#2180,.F.);
#3146=ORIENTED_EDGE('',*,*,#2186,.T.);
#3147=ORIENTED_EDGE('',*,*,#2187,.T.);
#3148=ORIENTED_EDGE('',*,*,#2187,.F.);
#3149=ORIENTED_EDGE('',*,*,#2185,.F.);
#3150=CYLINDRICAL_SURFACE('',#3538,1.225);
#3151=CYLINDRICAL_SURFACE('',#3541,1.225);
#3152=CYLINDRICAL_SURFACE('',#3544,1.65);
#3153=CYLINDRICAL_SURFACE('',#3567,1.);
#3154=CYLINDRICAL_SURFACE('',#3568,1.);
#3155=CYLINDRICAL_SURFACE('',#3569,0.2);
#3156=CYLINDRICAL_SURFACE('',#3570,0.2);
#3157=CYLINDRICAL_SURFACE('',#3578,3.075);
#3158=CYLINDRICAL_SURFACE('',#3581,4.1);
#3159=CYLINDRICAL_SURFACE('',#3584,4.1);
#3160=CYLINDRICAL_SURFACE('',#3616,0.5);
#3161=CYLINDRICAL_SURFACE('',#3617,0.5);
#3162=CYLINDRICAL_SURFACE('',#3618,0.5);
#3163=CYLINDRICAL_SURFACE('',#3619,0.5);
#3164=CYLINDRICAL_SURFACE('',#3620,0.5);
#3165=CYLINDRICAL_SURFACE('',#3621,0.5);
#3166=CYLINDRICAL_SURFACE('',#3622,0.5);
#3167=CYLINDRICAL_SURFACE('',#3623,0.5);
#3168=CYLINDRICAL_SURFACE('',#3625,6.3);
#3169=CYLINDRICAL_SURFACE('',#3628,4.1);
#3170=CYLINDRICAL_SURFACE('',#3634,4.2);
#3171=CYLINDRICAL_SURFACE('',#3652,3.);
#3172=CYLINDRICAL_SURFACE('',#3659,1.);
#3173=CYLINDRICAL_SURFACE('',#3661,1.);
#3174=CYLINDRICAL_SURFACE('',#3663,2.3);
#3175=CYLINDRICAL_SURFACE('',#3669,1.14999999999999);
#3176=CYLINDRICAL_SURFACE('',#3671,1.49999999999999);
#3177=CYLINDRICAL_SURFACE('',#3677,3.);
#3178=CYLINDRICAL_SURFACE('',#3692,1.1);
#3179=CYLINDRICAL_SURFACE('',#3695,1.7);
#3180=CYLINDRICAL_SURFACE('',#3698,5.);
#3181=CYLINDRICAL_SURFACE('',#3713,1.7);
#3182=CYLINDRICAL_SURFACE('',#3714,1.5);
#3183=CYLINDRICAL_SURFACE('',#3715,6.);
#3184=CYLINDRICAL_SURFACE('',#3716,6.);
#3185=CYLINDRICAL_SURFACE('',#3717,1.1);
#3186=CYLINDRICAL_SURFACE('',#3722,1.15);
#3187=CYLINDRICAL_SURFACE('',#3729,0.0500000000000001);
#3188=CYLINDRICAL_SURFACE('',#3740,2.525);
#3189=CYLINDRICAL_SURFACE('',#3833,0.0500000000000001);
#3190=CYLINDRICAL_SURFACE('',#3858,0.0500000000000001);
#3191=CYLINDRICAL_SURFACE('',#3860,0.0499999999999999);
#3192=CYLINDRICAL_SURFACE('',#3865,0.0500000000000001);
#3193=CYLINDRICAL_SURFACE('',#3871,0.0499999999999999);
#3194=CYLINDRICAL_SURFACE('',#3885,0.0500000000000002);
#3195=CYLINDRICAL_SURFACE('',#3922,0.0500000000000001);
#3196=CYLINDRICAL_SURFACE('',#3924,0.0500000000000001);
#3197=CYLINDRICAL_SURFACE('',#3929,0.0500000000000001);
#3198=CYLINDRICAL_SURFACE('',#3931,0.0500000000000002);
#3199=CYLINDRICAL_SURFACE('',#3950,0.0500000000000001);
#3200=CYLINDRICAL_SURFACE('',#3952,0.0500000000000001);
#3201=CYLINDRICAL_SURFACE('',#3976,0.0499999999999999);
#3202=CYLINDRICAL_SURFACE('',#3981,0.0500000000000001);
#3203=CYLINDRICAL_SURFACE('',#3983,0.0500000000000001);
#3204=CYLINDRICAL_SURFACE('',#3988,0.0499999999999999);
#3205=CYLINDRICAL_SURFACE('',#4010,0.0500000000000001);
#3206=ADVANCED_FACE('',(#294),#3150,.F.);
#3207=ADVANCED_FACE('',(#295),#3151,.F.);
#3208=ADVANCED_FACE('',(#296),#3152,.F.);
#3209=ADVANCED_FACE('',(#297),#224,.F.);
#3210=ADVANCED_FACE('',(#298),#225,.F.);
#3211=ADVANCED_FACE('',(#299),#226,.F.);
#3212=ADVANCED_FACE('',(#300),#227,.F.);
#3213=ADVANCED_FACE('',(#301,#197,#198),#228,.F.);
#3214=ADVANCED_FACE('',(#302,#199),#229,.F.);
#3215=ADVANCED_FACE('',(#303),#230,.F.);
#3216=ADVANCED_FACE('',(#304),#231,.T.);
#3217=ADVANCED_FACE('',(#305),#232,.F.);
#3218=ADVANCED_FACE('',(#306),#233,.F.);
#3219=ADVANCED_FACE('',(#307,#200),#234,.F.);
#3220=ADVANCED_FACE('',(#308,#201,#202),#235,.F.);
#3221=ADVANCED_FACE('',(#309),#3153,.T.);
#3222=ADVANCED_FACE('',(#310),#3154,.T.);
#3223=ADVANCED_FACE('',(#311),#3155,.F.);
#3224=ADVANCED_FACE('',(#312),#3156,.F.);
#3225=ADVANCED_FACE('',(#313),#236,.F.);
#3226=ADVANCED_FACE('',(#314),#237,.F.);
#3227=ADVANCED_FACE('',(#315),#238,.F.);
#3228=ADVANCED_FACE('',(#316),#239,.F.);
#3229=ADVANCED_FACE('',(#317),#240,.F.);
#3230=ADVANCED_FACE('',(#318),#241,.F.);
#3231=ADVANCED_FACE('',(#319),#3157,.F.);
#3232=ADVANCED_FACE('',(#320),#3158,.T.);
#3233=ADVANCED_FACE('',(#321),#3159,.T.);
#3234=ADVANCED_FACE('',(#322,#203),#242,.F.);
#3235=ADVANCED_FACE('',(#323),#243,.F.);
#3236=ADVANCED_FACE('',(#324),#244,.F.);
#3237=ADVANCED_FACE('',(#325),#245,.F.);
#3238=ADVANCED_FACE('',(#326),#246,.F.);
#3239=ADVANCED_FACE('',(#327,#204),#247,.T.);
#3240=ADVANCED_FACE('',(#328,#205),#248,.F.);
#3241=ADVANCED_FACE('',(#329),#249,.T.);
#3242=ADVANCED_FACE('',(#330),#250,.T.);
#3243=ADVANCED_FACE('',(#331),#251,.T.);
#3244=ADVANCED_FACE('',(#332),#252,.T.);
#3245=ADVANCED_FACE('',(#333,#206),#253,.T.);
#3246=ADVANCED_FACE('',(#334,#207),#254,.F.);
#3247=ADVANCED_FACE('',(#335),#3160,.T.);
#3248=ADVANCED_FACE('',(#336),#3161,.T.);
#3249=ADVANCED_FACE('',(#337),#3162,.T.);
#3250=ADVANCED_FACE('',(#338),#3163,.T.);
#3251=ADVANCED_FACE('',(#339),#3164,.T.);
#3252=ADVANCED_FACE('',(#340),#3165,.T.);
#3253=ADVANCED_FACE('',(#341),#3166,.T.);
#3254=ADVANCED_FACE('',(#342),#3167,.T.);
#3255=ADVANCED_FACE('',(#343),#3168,.T.);
#3256=ADVANCED_FACE('',(#344),#3169,.F.);
#3257=ADVANCED_FACE('',(#345,#208),#255,.F.);
#3258=ADVANCED_FACE('',(#346,#209),#256,.F.);
#3259=ADVANCED_FACE('',(#347),#3170,.F.);
#3260=ADVANCED_FACE('',(#348),#257,.F.);
#3261=ADVANCED_FACE('',(#349),#258,.F.);
#3262=ADVANCED_FACE('',(#350),#259,.F.);
#3263=ADVANCED_FACE('',(#351),#260,.F.);
#3264=ADVANCED_FACE('',(#352,#210),#261,.T.);
#3265=ADVANCED_FACE('',(#353,#211),#262,.F.);
#3266=ADVANCED_FACE('',(#354),#263,.F.);
#3267=ADVANCED_FACE('',(#355),#264,.F.);
#3268=ADVANCED_FACE('',(#356),#265,.F.);
#3269=ADVANCED_FACE('',(#357),#266,.F.);
#3270=ADVANCED_FACE('',(#358),#267,.F.);
#3271=ADVANCED_FACE('',(#359),#268,.F.);
#3272=ADVANCED_FACE('',(#360),#269,.F.);
#3273=ADVANCED_FACE('',(#361),#270,.F.);
#3274=ADVANCED_FACE('',(#362),#155,.T.);
#3275=ADVANCED_FACE('',(#363),#156,.T.);
#3276=ADVANCED_FACE('',(#364,#212,#213),#3171,.T.);
#3277=ADVANCED_FACE('',(#365),#3172,.F.);
#3278=ADVANCED_FACE('',(#366),#3173,.F.);
#3279=ADVANCED_FACE('',(#367),#3174,.T.);
#3280=ADVANCED_FACE('',(#368),#135,.T.);
#3281=ADVANCED_FACE('',(#369),#3175,.T.);
#3282=ADVANCED_FACE('',(#370),#3176,.T.);
#3283=ADVANCED_FACE('',(#371),#136,.T.);
#3284=ADVANCED_FACE('',(#372),#3177,.T.);
#3285=ADVANCED_FACE('',(#373,#214),#271,.F.);
#3286=ADVANCED_FACE('',(#374,#215),#272,.F.);
#3287=ADVANCED_FACE('',(#375,#216),#273,.F.);
#3288=ADVANCED_FACE('',(#376),#274,.F.);
#3289=ADVANCED_FACE('',(#377,#217),#275,.T.);
#3290=ADVANCED_FACE('',(#378,#218),#276,.T.);
#3291=ADVANCED_FACE('',(#379),#157,.T.);
#3292=ADVANCED_FACE('',(#380),#158,.T.);
#3293=ADVANCED_FACE('',(#381),#277,.F.);
#3294=ADVANCED_FACE('',(#382,#219),#278,.F.);
#3295=ADVANCED_FACE('',(#383),#279,.F.);
#3296=ADVANCED_FACE('',(#384,#220),#280,.F.);
#3297=ADVANCED_FACE('',(#385),#281,.F.);
#3298=ADVANCED_FACE('',(#386),#3178,.T.);
#3299=ADVANCED_FACE('',(#387),#3179,.F.);
#3300=ADVANCED_FACE('',(#388),#3180,.T.);
#3301=ADVANCED_FACE('',(#389),#282,.T.);
#3302=ADVANCED_FACE('',(#390),#283,.F.);
#3303=ADVANCED_FACE('',(#391),#3181,.F.);
#3304=ADVANCED_FACE('',(#392),#3182,.T.);
#3305=ADVANCED_FACE('',(#393),#3183,.T.);
#3306=ADVANCED_FACE('',(#394),#3184,.T.);
#3307=ADVANCED_FACE('',(#395),#3185,.T.);
#3308=ADVANCED_FACE('',(#396),#137,.F.);
#3309=ADVANCED_FACE('',(#397),#3186,.F.);
#3310=ADVANCED_FACE('',(#398),#97,.T.);
#3311=ADVANCED_FACE('',(#399),#3187,.T.);
#3312=ADVANCED_FACE('',(#400),#98,.T.);
#3313=ADVANCED_FACE('',(#401),#50,.T.);
#3314=ADVANCED_FACE('',(#402),#3188,.T.);
#3315=ADVANCED_FACE('',(#403),#51,.T.);
#3316=ADVANCED_FACE('',(#404),#52,.T.);
#3317=ADVANCED_FACE('',(#405),#53,.T.);
#3318=ADVANCED_FACE('',(#406),#54,.T.);
#3319=ADVANCED_FACE('',(#407),#284,.T.);
#3320=ADVANCED_FACE('',(#408),#285,.T.);
#3321=ADVANCED_FACE('',(#409),#286,.T.);
#3322=ADVANCED_FACE('',(#410),#287,.T.);
#3323=ADVANCED_FACE('',(#411),#288,.T.);
#3324=ADVANCED_FACE('',(#412),#289,.T.);
#3325=ADVANCED_FACE('',(#413,#221),#290,.T.);
#3326=ADVANCED_FACE('',(#414,#222),#291,.F.);
#3327=ADVANCED_FACE('',(#415),#55,.T.);
#3328=ADVANCED_FACE('',(#416),#56,.T.);
#3329=ADVANCED_FACE('',(#417),#57,.T.);
#3330=ADVANCED_FACE('',(#418),#58,.T.);
#3331=ADVANCED_FACE('',(#419),#59,.T.);
#3332=ADVANCED_FACE('',(#420),#60,.T.);
#3333=ADVANCED_FACE('',(#421),#61,.T.);
#3334=ADVANCED_FACE('',(#422),#62,.T.);
#3335=ADVANCED_FACE('',(#423),#63,.T.);
#3336=ADVANCED_FACE('',(#424),#3189,.T.);
#3337=ADVANCED_FACE('',(#425),#99,.T.);
#3338=ADVANCED_FACE('',(#426),#100,.T.);
#3339=ADVANCED_FACE('',(#427),#101,.T.);
#3340=ADVANCED_FACE('',(#428),#102,.T.);
#3341=ADVANCED_FACE('',(#429),#64,.T.);
#3342=ADVANCED_FACE('',(#430),#65,.T.);
#3343=ADVANCED_FACE('',(#431),#66,.T.);
#3344=ADVANCED_FACE('',(#432),#67,.T.);
#3345=ADVANCED_FACE('',(#433),#103,.T.);
#3346=ADVANCED_FACE('',(#434),#104,.T.);
#3347=ADVANCED_FACE('',(#435),#3190,.T.);
#3348=ADVANCED_FACE('',(#436),#3191,.T.);
#3349=ADVANCED_FACE('',(#437),#105,.T.);
#3350=ADVANCED_FACE('',(#438),#3192,.T.);
#3351=ADVANCED_FACE('',(#439),#106,.T.);
#3352=ADVANCED_FACE('',(#440),#3193,.T.);
#3353=ADVANCED_FACE('',(#441),#68,.T.);
#3354=ADVANCED_FACE('',(#442),#69,.T.);
#3355=ADVANCED_FACE('',(#443),#70,.T.);
#3356=ADVANCED_FACE('',(#444),#71,.T.);
#3357=ADVANCED_FACE('',(#445),#72,.T.);
#3358=ADVANCED_FACE('',(#446),#73,.T.);
#3359=ADVANCED_FACE('',(#447),#3194,.T.);
#3360=ADVANCED_FACE('',(#448),#107,.T.);
#3361=ADVANCED_FACE('',(#449),#108,.T.);
#3362=ADVANCED_FACE('',(#450),#109,.T.);
#3363=ADVANCED_FACE('',(#451),#110,.T.);
#3364=ADVANCED_FACE('',(#452),#111,.T.);
#3365=ADVANCED_FACE('',(#453),#112,.T.);
#3366=ADVANCED_FACE('',(#454),#113,.T.);
#3367=ADVANCED_FACE('',(#455),#74,.T.);
#3368=ADVANCED_FACE('',(#456),#75,.T.);
#3369=ADVANCED_FACE('',(#457),#76,.T.);
#3370=ADVANCED_FACE('',(#458),#77,.T.);
#3371=ADVANCED_FACE('',(#459),#78,.T.);
#3372=ADVANCED_FACE('',(#460),#79,.T.);
#3373=ADVANCED_FACE('',(#461),#114,.T.);
#3374=ADVANCED_FACE('',(#462),#115,.T.);
#3375=ADVANCED_FACE('',(#463),#116,.T.);
#3376=ADVANCED_FACE('',(#464),#3195,.T.);
#3377=ADVANCED_FACE('',(#465),#3196,.T.);
#3378=ADVANCED_FACE('',(#466),#117,.T.);
#3379=ADVANCED_FACE('',(#467),#3197,.T.);
#3380=ADVANCED_FACE('',(#468),#3198,.T.);
#3381=ADVANCED_FACE('',(#469),#118,.T.);
#3382=ADVANCED_FACE('',(#470),#80,.T.);
#3383=ADVANCED_FACE('',(#471),#81,.T.);
#3384=ADVANCED_FACE('',(#472),#82,.T.);
#3385=ADVANCED_FACE('',(#473),#83,.T.);
#3386=ADVANCED_FACE('',(#474),#84,.T.);
#3387=ADVANCED_FACE('',(#475),#85,.T.);
#3388=ADVANCED_FACE('',(#476),#86,.T.);
#3389=ADVANCED_FACE('',(#477),#3199,.T.);
#3390=ADVANCED_FACE('',(#478),#3200,.T.);
#3391=ADVANCED_FACE('',(#479),#119,.T.);
#3392=ADVANCED_FACE('',(#480),#120,.T.);
#3393=ADVANCED_FACE('',(#481),#121,.T.);
#3394=ADVANCED_FACE('',(#482),#122,.T.);
#3395=ADVANCED_FACE('',(#483),#123,.T.);
#3396=ADVANCED_FACE('',(#484),#124,.T.);
#3397=ADVANCED_FACE('',(#485),#125,.T.);
#3398=ADVANCED_FACE('',(#486),#87,.T.);
#3399=ADVANCED_FACE('',(#487),#88,.T.);
#3400=ADVANCED_FACE('',(#488),#89,.T.);
#3401=ADVANCED_FACE('',(#489),#90,.T.);
#3402=ADVANCED_FACE('',(#490),#3201,.T.);
#3403=ADVANCED_FACE('',(#491),#126,.T.);
#3404=ADVANCED_FACE('',(#492),#3202,.T.);
#3405=ADVANCED_FACE('',(#493),#3203,.T.);
#3406=ADVANCED_FACE('',(#494),#127,.T.);
#3407=ADVANCED_FACE('',(#495),#3204,.T.);
#3408=ADVANCED_FACE('',(#496),#91,.T.);
#3409=ADVANCED_FACE('',(#497),#92,.T.);
#3410=ADVANCED_FACE('',(#498),#93,.T.);
#3411=ADVANCED_FACE('',(#499),#94,.T.);
#3412=ADVANCED_FACE('',(#500),#128,.T.);
#3413=ADVANCED_FACE('',(#501),#129,.T.);
#3414=ADVANCED_FACE('',(#502),#130,.T.);
#3415=ADVANCED_FACE('',(#503),#131,.T.);
#3416=ADVANCED_FACE('',(#504),#95,.T.);
#3417=ADVANCED_FACE('',(#505),#96,.T.);
#3418=ADVANCED_FACE('',(#506),#3205,.T.);
#3419=ADVANCED_FACE('',(#507),#292,.T.);
#3420=ADVANCED_FACE('',(#508),#132,.T.);
#3421=ADVANCED_FACE('',(#509),#133,.T.);
#3422=ADVANCED_FACE('',(#510,#223),#134,.T.);
#3423=ADVANCED_FACE('',(#511),#47,.F.);
#3424=ADVANCED_FACE('',(#512),#48,.F.);
#3425=ADVANCED_FACE('',(#513),#293,.F.);
#3426=CLOSED_SHELL('',(#3206,#3207,#3208,#3209,#3210,#3211,#3212,#3213,
#3214,#3215,#3216,#3217,#3218,#3219,#3220,#3221,#3222,#3223,#3224,#3225,
#3226,#3227,#3228,#3229,#3230));
#3427=CLOSED_SHELL('',(#3231,#3232,#3233,#3234,#3235,#3236,#3237,#3238,
#3239,#3240,#3241,#3242,#3243,#3244,#3245,#3246,#3247,#3248,#3249,#3250,
#3251,#3252,#3253,#3254));
#3428=CLOSED_SHELL('',(#3255,#3256,#3257,#3258));
#3429=CLOSED_SHELL('',(#3259,#3260,#3261,#3262,#3263,#3264,#3265,#3266,
#3267,#3268,#3269,#3270,#3271,#3272,#3273));
#3430=CLOSED_SHELL('',(#3274,#3275,#3276,#3277,#3278,#3279,#3280,#3281,
#3282,#3283,#3284,#3285,#3286,#3287,#3288,#3289,#3290,#3291,#3292,#3293,
#3294,#3295,#3296,#3297));
#3431=CLOSED_SHELL('',(#3298,#3299,#3300,#3301,#3302,#3303,#3304,#3305,
#3306,#3307));
#3432=CLOSED_SHELL('',(#3308,#3309,#3310,#3311,#3312,#3313,#3314,#3315,
#3316,#3317,#3318,#3319,#3320,#3321,#3322,#3323,#3324,#3325,#3326,#3327,
#3328,#3329,#3330,#3331,#3332,#3333,#3334,#3335,#3336,#3337,#3338,#3339,
#3340,#3341,#3342,#3343,#3344,#3345,#3346,#3347,#3348,#3349,#3350,#3351,
#3352,#3353,#3354,#3355,#3356,#3357,#3358,#3359,#3360,#3361,#3362,#3363,
#3364,#3365,#3366,#3367,#3368,#3369,#3370,#3371,#3372,#3373,#3374,#3375,
#3376,#3377,#3378,#3379,#3380,#3381,#3382,#3383,#3384,#3385,#3386,#3387,
#3388,#3389,#3390,#3391,#3392,#3393,#3394,#3395,#3396,#3397,#3398,#3399,
#3400,#3401,#3402,#3403,#3404,#3405,#3406,#3407,#3408,#3409,#3410,#3411,
#3412,#3413,#3414,#3415,#3416,#3417,#3418,#3419));
#3433=CLOSED_SHELL('',(#3420));
#3434=CLOSED_SHELL('',(#3421));
#3435=CLOSED_SHELL('',(#3422,#3423,#3424,#3425));
#3436=DERIVED_UNIT_ELEMENT(#3454,1.);
#3437=DERIVED_UNIT_ELEMENT(#10553,-3.);
#3438=DERIVED_UNIT_ELEMENT(#3454,1.);
#3439=DERIVED_UNIT_ELEMENT(#10553,-3.);
#3440=DERIVED_UNIT_ELEMENT(#3454,1.);
#3441=DERIVED_UNIT_ELEMENT(#10553,-3.);
#3442=DERIVED_UNIT_ELEMENT(#3454,1.);
#3443=DERIVED_UNIT_ELEMENT(#10553,-3.);
#3444=DERIVED_UNIT_ELEMENT(#3454,1.);
#3445=DERIVED_UNIT_ELEMENT(#10553,-3.);
#3446=DERIVED_UNIT_ELEMENT(#3454,1.);
#3447=DERIVED_UNIT_ELEMENT(#10553,-3.);
#3448=DERIVED_UNIT_ELEMENT(#3454,1.);
#3449=DERIVED_UNIT_ELEMENT(#10553,-3.);
#3450=DERIVED_UNIT_ELEMENT(#3454,1.);
#3451=DERIVED_UNIT_ELEMENT(#10553,-3.);
#3452=DERIVED_UNIT_ELEMENT(#3454,1.);
#3453=DERIVED_UNIT_ELEMENT(#10553,-3.);
#3454=(
MASS_UNIT()
NAMED_UNIT(*)
SI_UNIT(.KILO.,.GRAM.)
);
#3455=DERIVED_UNIT((#3436,#3437));
#3456=DERIVED_UNIT((#3438,#3439));
#3457=DERIVED_UNIT((#3440,#3441));
#3458=DERIVED_UNIT((#3442,#3443));
#3459=DERIVED_UNIT((#3444,#3445));
#3460=DERIVED_UNIT((#3446,#3447));
#3461=DERIVED_UNIT((#3448,#3449));
#3462=DERIVED_UNIT((#3450,#3451));
#3463=DERIVED_UNIT((#3452,#3453));
#3464=MEASURE_REPRESENTATION_ITEM('density measure',
POSITIVE_RATIO_MEASURE(7850.),#3455);
#3465=MEASURE_REPRESENTATION_ITEM('density measure',
POSITIVE_RATIO_MEASURE(7850.),#3456);
#3466=MEASURE_REPRESENTATION_ITEM('density measure',
POSITIVE_RATIO_MEASURE(7850.),#3457);
#3467=MEASURE_REPRESENTATION_ITEM('density measure',
POSITIVE_RATIO_MEASURE(7850.),#3458);
#3468=MEASURE_REPRESENTATION_ITEM('density measure',
POSITIVE_RATIO_MEASURE(7850.),#3459);
#3469=MEASURE_REPRESENTATION_ITEM('density measure',
POSITIVE_RATIO_MEASURE(7850.),#3460);
#3470=MEASURE_REPRESENTATION_ITEM('density measure',
POSITIVE_RATIO_MEASURE(7850.),#3461);
#3471=MEASURE_REPRESENTATION_ITEM('density measure',
POSITIVE_RATIO_MEASURE(7850.),#3462);
#3472=MEASURE_REPRESENTATION_ITEM('density measure',
POSITIVE_RATIO_MEASURE(7850.),#3463);
#3473=PROPERTY_DEFINITION_REPRESENTATION(#3518,#3491);
#3474=PROPERTY_DEFINITION_REPRESENTATION(#3519,#3492);
#3475=PROPERTY_DEFINITION_REPRESENTATION(#3520,#3493);
#3476=PROPERTY_DEFINITION_REPRESENTATION(#3521,#3494);
#3477=PROPERTY_DEFINITION_REPRESENTATION(#3522,#3495);
#3478=PROPERTY_DEFINITION_REPRESENTATION(#3523,#3496);
#3479=PROPERTY_DEFINITION_REPRESENTATION(#3524,#3497);
#3480=PROPERTY_DEFINITION_REPRESENTATION(#3525,#3498);
#3481=PROPERTY_DEFINITION_REPRESENTATION(#3526,#3499);
#3482=PROPERTY_DEFINITION_REPRESENTATION(#3527,#3500);
#3483=PROPERTY_DEFINITION_REPRESENTATION(#3528,#3501);
#3484=PROPERTY_DEFINITION_REPRESENTATION(#3529,#3502);
#3485=PROPERTY_DEFINITION_REPRESENTATION(#3530,#3503);
#3486=PROPERTY_DEFINITION_REPRESENTATION(#3531,#3504);
#3487=PROPERTY_DEFINITION_REPRESENTATION(#3532,#3505);
#3488=PROPERTY_DEFINITION_REPRESENTATION(#3533,#3506);
#3489=PROPERTY_DEFINITION_REPRESENTATION(#3534,#3507);
#3490=PROPERTY_DEFINITION_REPRESENTATION(#3535,#3508);
#3491=REPRESENTATION('material name',(#3509),#10542);
#3492=REPRESENTATION('density',(#3464),#10542);
#3493=REPRESENTATION('material name',(#3510),#10543);
#3494=REPRESENTATION('density',(#3465),#10543);
#3495=REPRESENTATION('material name',(#3511),#10544);
#3496=REPRESENTATION('density',(#3466),#10544);
#3497=REPRESENTATION('material name',(#3512),#10545);
#3498=REPRESENTATION('density',(#3467),#10545);
#3499=REPRESENTATION('material name',(#3513),#10546);
#3500=REPRESENTATION('density',(#3468),#10546);
#3501=REPRESENTATION('material name',(#3514),#10547);
#3502=REPRESENTATION('density',(#3469),#10547);
#3503=REPRESENTATION('material name',(#3515),#10548);
#3504=REPRESENTATION('density',(#3470),#10548);
#3505=REPRESENTATION('material name',(#3516),#10549);
#3506=REPRESENTATION('density',(#3471),#10549);
#3507=REPRESENTATION('material name',(#3517),#10550);
#3508=REPRESENTATION('density',(#3472),#10550);
#3509=DESCRIPTIVE_REPRESENTATION_ITEM('Steel','Steel');
#3510=DESCRIPTIVE_REPRESENTATION_ITEM('Steel','Steel');
#3511=DESCRIPTIVE_REPRESENTATION_ITEM('Steel','Steel');
#3512=DESCRIPTIVE_REPRESENTATION_ITEM('Steel','Steel');
#3513=DESCRIPTIVE_REPRESENTATION_ITEM('Steel','Steel');
#3514=DESCRIPTIVE_REPRESENTATION_ITEM('Steel','Steel');
#3515=DESCRIPTIVE_REPRESENTATION_ITEM('Steel','Steel');
#3516=DESCRIPTIVE_REPRESENTATION_ITEM('Steel','Steel');
#3517=DESCRIPTIVE_REPRESENTATION_ITEM('Steel','Steel');
#3518=PROPERTY_DEFINITION('material property','material name',#10597);
#3519=PROPERTY_DEFINITION('material property','density of part',#10597);
#3520=PROPERTY_DEFINITION('material property','material name',#10598);
#3521=PROPERTY_DEFINITION('material property','density of part',#10598);
#3522=PROPERTY_DEFINITION('material property','material name',#10599);
#3523=PROPERTY_DEFINITION('material property','density of part',#10599);
#3524=PROPERTY_DEFINITION('material property','material name',#10600);
#3525=PROPERTY_DEFINITION('material property','density of part',#10600);
#3526=PROPERTY_DEFINITION('material property','material name',#10601);
#3527=PROPERTY_DEFINITION('material property','density of part',#10601);
#3528=PROPERTY_DEFINITION('material property','material name',#10602);
#3529=PROPERTY_DEFINITION('material property','density of part',#10602);
#3530=PROPERTY_DEFINITION('material property','material name',#10603);
#3531=PROPERTY_DEFINITION('material property','density of part',#10603);
#3532=PROPERTY_DEFINITION('material property','material name',#10604);
#3533=PROPERTY_DEFINITION('material property','density of part',#10604);
#3534=PROPERTY_DEFINITION('material property','material name',#10605);
#3535=PROPERTY_DEFINITION('material property','density of part',#10605);
#3536=AXIS2_PLACEMENT_3D('',#5233,#4036,#4037);
#3537=AXIS2_PLACEMENT_3D('',#5234,#4038,#4039);
#3538=AXIS2_PLACEMENT_3D('',#5235,#4040,#4041);
#3539=AXIS2_PLACEMENT_3D('',#5237,#4042,#4043);
#3540=AXIS2_PLACEMENT_3D('',#5240,#4045,#4046);
#3541=AXIS2_PLACEMENT_3D('',#5241,#4047,#4048);
#3542=AXIS2_PLACEMENT_3D('',#5243,#4049,#4050);
#3543=AXIS2_PLACEMENT_3D('',#5246,#4052,#4053);
#3544=AXIS2_PLACEMENT_3D('',#5247,#4054,#4055);
#3545=AXIS2_PLACEMENT_3D('',#5249,#4056,#4057);
#3546=AXIS2_PLACEMENT_3D('',#5252,#4059,#4060);
#3547=AXIS2_PLACEMENT_3D('',#5253,#4061,#4062);
#3548=AXIS2_PLACEMENT_3D('',#5262,#4067,#4068);
#3549=AXIS2_PLACEMENT_3D('',#5271,#4073,#4074);
#3550=AXIS2_PLACEMENT_3D('',#5280,#4079,#4080);
#3551=AXIS2_PLACEMENT_3D('',#5289,#4085,#4086);
#3552=AXIS2_PLACEMENT_3D('',#5300,#4093,#4094);
#3553=AXIS2_PLACEMENT_3D('',#5309,#4099,#4100);
#3554=AXIS2_PLACEMENT_3D('',#5320,#4107,#4108);
#3555=AXIS2_PLACEMENT_3D('',#5321,#4109,#4110);
#3556=AXIS2_PLACEMENT_3D('',#5322,#4111,#4112);
#3557=AXIS2_PLACEMENT_3D('',#5326,#4114,#4115);
#3558=AXIS2_PLACEMENT_3D('',#5330,#4117,#4118);
#3559=AXIS2_PLACEMENT_3D('',#5332,#4120,#4121);
#3560=AXIS2_PLACEMENT_3D('',#5333,#4122,#4123);
#3561=AXIS2_PLACEMENT_3D('',#5337,#4125,#4126);
#3562=AXIS2_PLACEMENT_3D('',#5341,#4128,#4129);
#3563=AXIS2_PLACEMENT_3D('',#5343,#4131,#4132);
#3564=AXIS2_PLACEMENT_3D('',#5344,#4133,#4134);
#3565=AXIS2_PLACEMENT_3D('',#5351,#4139,#4140);
#3566=AXIS2_PLACEMENT_3D('',#5354,#4143,#4144);
#3567=AXIS2_PLACEMENT_3D('',#5361,#4149,#4150);
#3568=AXIS2_PLACEMENT_3D('',#5362,#4151,#4152);
#3569=AXIS2_PLACEMENT_3D('',#5363,#4153,#4154);
#3570=AXIS2_PLACEMENT_3D('',#5364,#4155,#4156);
#3571=AXIS2_PLACEMENT_3D('',#5365,#4157,#4158);
#3572=AXIS2_PLACEMENT_3D('',#5367,#4160,#4161);
#3573=AXIS2_PLACEMENT_3D('',#5369,#4163,#4164);
#3574=AXIS2_PLACEMENT_3D('',#5370,#4165,#4166);
#3575=AXIS2_PLACEMENT_3D('',#5372,#4168,#4169);
#3576=AXIS2_PLACEMENT_3D('',#5374,#4171,#4172);
#3577=AXIS2_PLACEMENT_3D('',#5375,#4173,#4174);
#3578=AXIS2_PLACEMENT_3D('',#5376,#4175,#4176);
#3579=AXIS2_PLACEMENT_3D('',#5378,#4177,#4178);
#3580=AXIS2_PLACEMENT_3D('',#5381,#4180,#4181);
#3581=AXIS2_PLACEMENT_3D('',#5382,#4182,#4183);
#3582=AXIS2_PLACEMENT_3D('',#5384,#4184,#4185);
#3583=AXIS2_PLACEMENT_3D('',#5387,#4187,#4188);
#3584=AXIS2_PLACEMENT_3D('',#5388,#4189,#4190);
#3585=AXIS2_PLACEMENT_3D('',#5390,#4191,#4192);
#3586=AXIS2_PLACEMENT_3D('',#5393,#4194,#4195);
#3587=AXIS2_PLACEMENT_3D('',#5394,#4196,#4197);
#3588=AXIS2_PLACEMENT_3D('',#5395,#4198,#4199);
#3589=AXIS2_PLACEMENT_3D('',#5404,#4204,#4205);
#3590=AXIS2_PLACEMENT_3D('',#5413,#4210,#4211);
#3591=AXIS2_PLACEMENT_3D('',#5422,#4216,#4217);
#3592=AXIS2_PLACEMENT_3D('',#5431,#4222,#4223);
#3593=AXIS2_PLACEMENT_3D('',#5432,#4224,#4225);
#3594=AXIS2_PLACEMENT_3D('',#5433,#4226,#4227);
#3595=AXIS2_PLACEMENT_3D('',#5434,#4228,#4229);
#3596=AXIS2_PLACEMENT_3D('',#5435,#4230,#4231);
#3597=AXIS2_PLACEMENT_3D('',#5436,#4232,#4233);
#3598=AXIS2_PLACEMENT_3D('',#5437,#4234,#4235);
#3599=AXIS2_PLACEMENT_3D('',#5438,#4236,#4237);
#3600=AXIS2_PLACEMENT_3D('',#5439,#4238,#4239);
#3601=AXIS2_PLACEMENT_3D('',#5440,#4240,#4241);
#3602=AXIS2_PLACEMENT_3D('',#5441,#4242,#4243);
#3603=AXIS2_PLACEMENT_3D('',#5450,#4248,#4249);
#3604=AXIS2_PLACEMENT_3D('',#5459,#4254,#4255);
#3605=AXIS2_PLACEMENT_3D('',#5468,#4260,#4261);
#3606=AXIS2_PLACEMENT_3D('',#5477,#4266,#4267);
#3607=AXIS2_PLACEMENT_3D('',#5478,#4268,#4269);
#3608=AXIS2_PLACEMENT_3D('',#5479,#4270,#4271);
#3609=AXIS2_PLACEMENT_3D('',#5480,#4272,#4273);
#3610=AXIS2_PLACEMENT_3D('',#5481,#4274,#4275);
#3611=AXIS2_PLACEMENT_3D('',#5482,#4276,#4277);
#3612=AXIS2_PLACEMENT_3D('',#5483,#4278,#4279);
#3613=AXIS2_PLACEMENT_3D('',#5484,#4280,#4281);
#3614=AXIS2_PLACEMENT_3D('',#5485,#4282,#4283);
#3615=AXIS2_PLACEMENT_3D('',#5486,#4284,#4285);
#3616=AXIS2_PLACEMENT_3D('',#5487,#4286,#4287);
#3617=AXIS2_PLACEMENT_3D('',#5488,#4288,#4289);
#3618=AXIS2_PLACEMENT_3D('',#5489,#4290,#4291);
#3619=AXIS2_PLACEMENT_3D('',#5490,#4292,#4293);
#3620=AXIS2_PLACEMENT_3D('',#5491,#4294,#4295);
#3621=AXIS2_PLACEMENT_3D('',#5492,#4296,#4297);
#3622=AXIS2_PLACEMENT_3D('',#5493,#4298,#4299);
#3623=AXIS2_PLACEMENT_3D('',#5494,#4300,#4301);
#3624=AXIS2_PLACEMENT_3D('',#5495,#4302,#4303);
#3625=AXIS2_PLACEMENT_3D('',#5496,#4304,#4305);
#3626=AXIS2_PLACEMENT_3D('',#5498,#4306,#4307);
#3627=AXIS2_PLACEMENT_3D('',#5501,#4309,#4310);
#3628=AXIS2_PLACEMENT_3D('',#5502,#4311,#4312);
#3629=AXIS2_PLACEMENT_3D('',#5504,#4313,#4314);
#3630=AXIS2_PLACEMENT_3D('',#5507,#4316,#4317);
#3631=AXIS2_PLACEMENT_3D('',#5508,#4318,#4319);
#3632=AXIS2_PLACEMENT_3D('',#5509,#4320,#4321);
#3633=AXIS2_PLACEMENT_3D('',#5510,#4322,#4323);
#3634=AXIS2_PLACEMENT_3D('',#5511,#4324,#4325);
#3635=AXIS2_PLACEMENT_3D('',#5513,#4326,#4327);
#3636=AXIS2_PLACEMENT_3D('',#5516,#4329,#4330);
#3637=AXIS2_PLACEMENT_3D('',#5517,#4331,#4332);
#3638=AXIS2_PLACEMENT_3D('',#5526,#4337,#4338);
#3639=AXIS2_PLACEMENT_3D('',#5535,#4343,#4344);
#3640=AXIS2_PLACEMENT_3D('',#5544,#4349,#4350);
#3641=AXIS2_PLACEMENT_3D('',#5553,#4355,#4356);
#3642=AXIS2_PLACEMENT_3D('',#5566,#4365,#4366);
#3643=AXIS2_PLACEMENT_3D('',#5579,#4375,#4376);
#3644=AXIS2_PLACEMENT_3D('',#5581,#4378,#4379);
#3645=AXIS2_PLACEMENT_3D('',#5582,#4380,#4381);
#3646=AXIS2_PLACEMENT_3D('',#5584,#4383,#4384);
#3647=AXIS2_PLACEMENT_3D('',#5585,#4385,#4386);
#3648=AXIS2_PLACEMENT_3D('',#5587,#4388,#4389);
#3649=AXIS2_PLACEMENT_3D('',#5588,#4390,#4391);
#3650=AXIS2_PLACEMENT_3D('',#5590,#4393,#4394);
#3651=AXIS2_PLACEMENT_3D('',#5591,#4395,#4396);
#3652=AXIS2_PLACEMENT_3D('',#6690,#4401,#4402);
#3653=AXIS2_PLACEMENT_3D('',#6693,#4403,#4404);
#3654=AXIS2_PLACEMENT_3D('',#6697,#4406,#4407);
#3655=AXIS2_PLACEMENT_3D('',#6701,#4409,#4410);
#3656=AXIS2_PLACEMENT_3D('',#6704,#4412,#4413);
#3657=AXIS2_PLACEMENT_3D('',#6706,#4414,#4415);
#3658=AXIS2_PLACEMENT_3D('',#6710,#4417,#4418);
#3659=AXIS2_PLACEMENT_3D('',#6756,#4420,#4421);
#3660=AXIS2_PLACEMENT_3D('',#6759,#4423,#4424);
#3661=AXIS2_PLACEMENT_3D('',#6782,#4425,#4426);
#3662=AXIS2_PLACEMENT_3D('',#6784,#4427,#4428);
#3663=AXIS2_PLACEMENT_3D('',#6808,#4430,#4431);
#3664=AXIS2_PLACEMENT_3D('',#6810,#4432,#4433);
#3665=AXIS2_PLACEMENT_3D('',#6813,#4435,#4436);
#3666=AXIS2_PLACEMENT_3D('',#6814,#4437,#4438);
#3667=AXIS2_PLACEMENT_3D('',#6816,#4439,#4440);
#3668=AXIS2_PLACEMENT_3D('',#6819,#4442,#4443);
#3669=AXIS2_PLACEMENT_3D('',#6820,#4444,#4445);
#3670=AXIS2_PLACEMENT_3D('',#6822,#4446,#4447);
#3671=AXIS2_PLACEMENT_3D('',#6824,#4449,#4450);
#3672=AXIS2_PLACEMENT_3D('',#6826,#4451,#4452);
#3673=AXIS2_PLACEMENT_3D('',#6829,#4454,#4455);
#3674=AXIS2_PLACEMENT_3D('',#6830,#4456,#4457);
#3675=AXIS2_PLACEMENT_3D('',#6832,#4458,#4459);
#3676=AXIS2_PLACEMENT_3D('',#6835,#4461,#4462);
#3677=AXIS2_PLACEMENT_3D('',#6836,#4463,#4464);
#3678=AXIS2_PLACEMENT_3D('',#6838,#4465,#4466);
#3679=AXIS2_PLACEMENT_3D('',#6841,#4468,#4469);
#3680=AXIS2_PLACEMENT_3D('',#6842,#4470,#4471);
#3681=AXIS2_PLACEMENT_3D('',#6843,#4472,#4473);
#3682=AXIS2_PLACEMENT_3D('',#6844,#4474,#4475);
#3683=AXIS2_PLACEMENT_3D('',#6845,#4476,#4477);
#3684=AXIS2_PLACEMENT_3D('',#6846,#4478,#4479);
#3685=AXIS2_PLACEMENT_3D('',#6847,#4480,#4481);
#3686=AXIS2_PLACEMENT_3D('',#7832,#4482,#4483);
#3687=AXIS2_PLACEMENT_3D('',#7834,#4485,#4486);
#3688=AXIS2_PLACEMENT_3D('',#7836,#4488,#4489);
#3689=AXIS2_PLACEMENT_3D('',#7838,#4491,#4492);
#3690=AXIS2_PLACEMENT_3D('',#7840,#4494,#4495);
#3691=AXIS2_PLACEMENT_3D('',#7841,#4496,#4497);
#3692=AXIS2_PLACEMENT_3D('',#7842,#4498,#4499);
#3693=AXIS2_PLACEMENT_3D('',#7845,#4500,#4501);
#3694=AXIS2_PLACEMENT_3D('',#7849,#4503,#4504);
#3695=AXIS2_PLACEMENT_3D('',#7851,#4506,#4507);
#3696=AXIS2_PLACEMENT_3D('',#7854,#4508,#4509);
#3697=AXIS2_PLACEMENT_3D('',#7858,#4511,#4512);
#3698=AXIS2_PLACEMENT_3D('',#7860,#4514,#4515);
#3699=AXIS2_PLACEMENT_3D('',#7862,#4516,#4517);
#3700=AXIS2_PLACEMENT_3D('',#7865,#4519,#4520);
#3701=AXIS2_PLACEMENT_3D('',#7866,#4521,#4522);
#3702=AXIS2_PLACEMENT_3D('',#7868,#4523,#4524);
#3703=AXIS2_PLACEMENT_3D('',#7869,#4525,#4526);
#3704=AXIS2_PLACEMENT_3D('',#7871,#4527,#4528);
#3705=AXIS2_PLACEMENT_3D('',#7873,#4529,#4530);
#3706=AXIS2_PLACEMENT_3D('',#7874,#4531,#4532);
#3707=AXIS2_PLACEMENT_3D('',#7875,#4533,#4534);
#3708=AXIS2_PLACEMENT_3D('',#7877,#4535,#4536);
#3709=AXIS2_PLACEMENT_3D('',#7878,#4537,#4538);
#3710=AXIS2_PLACEMENT_3D('',#7880,#4539,#4540);
#3711=AXIS2_PLACEMENT_3D('',#7882,#4541,#4542);
#3712=AXIS2_PLACEMENT_3D('',#7883,#4543,#4544);
#3713=AXIS2_PLACEMENT_3D('',#7884,#4545,#4546);
#3714=AXIS2_PLACEMENT_3D('',#7887,#4549,#4550);
#3715=AXIS2_PLACEMENT_3D('',#7888,#4551,#4552);
#3716=AXIS2_PLACEMENT_3D('',#7890,#4554,#4555);
#3717=AXIS2_PLACEMENT_3D('',#7891,#4556,#4557);
#3718=AXIS2_PLACEMENT_3D('',#7892,#4558,#4559);
#3719=AXIS2_PLACEMENT_3D('',#7893,#4560,#4561);
#3720=AXIS2_PLACEMENT_3D('',#7895,#4562,#4563);
#3721=AXIS2_PLACEMENT_3D('',#7898,#4565,#4566);
#3722=AXIS2_PLACEMENT_3D('',#7899,#4567,#4568);
#3723=AXIS2_PLACEMENT_3D('',#7901,#4569,#4570);
#3724=AXIS2_PLACEMENT_3D('',#7903,#4572,#4573);
#3725=AXIS2_PLACEMENT_3D('',#7906,#4574,#4575);
#3726=AXIS2_PLACEMENT_3D('',#7908,#4576,#4577);
#3727=AXIS2_PLACEMENT_3D('',#7910,#4578,#4579);
#3728=AXIS2_PLACEMENT_3D('',#7911,#4580,#4581);
#3729=AXIS2_PLACEMENT_3D('',#7912,#4582,#4583);
#3730=AXIS2_PLACEMENT_3D('',#7915,#4584,#4585);
#3731=AXIS2_PLACEMENT_3D('',#7919,#4587,#4588);
#3732=AXIS2_PLACEMENT_3D('',#7921,#4590,#4591);
#3733=AXIS2_PLACEMENT_3D('',#7924,#4592,#4593);
#3734=AXIS2_PLACEMENT_3D('',#7926,#4594,#4595);
#3735=AXIS2_PLACEMENT_3D('',#7928,#4596,#4597);
#3736=AXIS2_PLACEMENT_3D('',#7929,#4598,#4599);
#3737=AXIS2_PLACEMENT_3D('',#7930,#4600,#4601);
#3738=AXIS2_PLACEMENT_3D('',#7932,#4602,#4603);
#3739=AXIS2_PLACEMENT_3D('',#7934,#4604,#4605);
#3740=AXIS2_PLACEMENT_3D('',#7935,#4606,#4607);
#3741=AXIS2_PLACEMENT_3D('',#7937,#4608,#4609);
#3742=AXIS2_PLACEMENT_3D('',#7939,#4611,#4612);
#3743=AXIS2_PLACEMENT_3D('',#7942,#4613,#4614);
#3744=AXIS2_PLACEMENT_3D('',#7944,#4615,#4616);
#3745=AXIS2_PLACEMENT_3D('',#7945,#4617,#4618);
#3746=AXIS2_PLACEMENT_3D('',#7946,#4619,#4620);
#3747=AXIS2_PLACEMENT_3D('',#7949,#4621,#4622);
#3748=AXIS2_PLACEMENT_3D('',#7951,#4623,#4624);
#3749=AXIS2_PLACEMENT_3D('',#7952,#4625,#4626);
#3750=AXIS2_PLACEMENT_3D('',#7953,#4627,#4628);
#3751=AXIS2_PLACEMENT_3D('',#7956,#4629,#4630);
#3752=AXIS2_PLACEMENT_3D('',#7958,#4631,#4632);
#3753=AXIS2_PLACEMENT_3D('',#7959,#4633,#4634);
#3754=AXIS2_PLACEMENT_3D('',#7960,#4635,#4636);
#3755=AXIS2_PLACEMENT_3D('',#7963,#4637,#4638);
#3756=AXIS2_PLACEMENT_3D('',#7965,#4639,#4640);
#3757=AXIS2_PLACEMENT_3D('',#7966,#4641,#4642);
#3758=AXIS2_PLACEMENT_3D('',#7967,#4643,#4644);
#3759=AXIS2_PLACEMENT_3D('',#7972,#4646,#4647);
#3760=AXIS2_PLACEMENT_3D('',#7976,#4649,#4650);
#3761=AXIS2_PLACEMENT_3D('',#7980,#4652,#4653);
#3762=AXIS2_PLACEMENT_3D('',#7983,#4655,#4656);
#3763=AXIS2_PLACEMENT_3D('',#7984,#4657,#4658);
#3764=AXIS2_PLACEMENT_3D('',#7987,#4659,#4660);
#3765=AXIS2_PLACEMENT_3D('',#7991,#4662,#4663);
#3766=AXIS2_PLACEMENT_3D('',#7995,#4665,#4666);
#3767=AXIS2_PLACEMENT_3D('',#7999,#4668,#4669);
#3768=AXIS2_PLACEMENT_3D('',#8001,#4671,#4672);
#3769=AXIS2_PLACEMENT_3D('',#8004,#4673,#4674);
#3770=AXIS2_PLACEMENT_3D('',#8008,#4676,#4677);
#3771=AXIS2_PLACEMENT_3D('',#8012,#4679,#4680);
#3772=AXIS2_PLACEMENT_3D('',#8016,#4682,#4683);
#3773=AXIS2_PLACEMENT_3D('',#8018,#4685,#4686);
#3774=AXIS2_PLACEMENT_3D('',#8021,#4687,#4688);
#3775=AXIS2_PLACEMENT_3D('',#8025,#4690,#4691);
#3776=AXIS2_PLACEMENT_3D('',#8029,#4693,#4694);
#3777=AXIS2_PLACEMENT_3D('',#8033,#4696,#4697);
#3778=AXIS2_PLACEMENT_3D('',#8035,#4699,#4700);
#3779=AXIS2_PLACEMENT_3D('',#8037,#4701,#4702);
#3780=AXIS2_PLACEMENT_3D('',#8041,#4704,#4705);
#3781=AXIS2_PLACEMENT_3D('',#8045,#4707,#4708);
#3782=AXIS2_PLACEMENT_3D('',#8048,#4710,#4711);
#3783=AXIS2_PLACEMENT_3D('',#8049,#4712,#4713);
#3784=AXIS2_PLACEMENT_3D('',#8052,#4714,#4715);
#3785=AXIS2_PLACEMENT_3D('',#8055,#4717,#4718);
#3786=AXIS2_PLACEMENT_3D('',#8057,#4719,#4720);
#3787=AXIS2_PLACEMENT_3D('',#8061,#4722,#4723);
#3788=AXIS2_PLACEMENT_3D('',#8063,#4725,#4726);
#3789=AXIS2_PLACEMENT_3D('',#8066,#4727,#4728);
#3790=AXIS2_PLACEMENT_3D('',#8070,#4730,#4731);
#3791=AXIS2_PLACEMENT_3D('',#8075,#4734,#4735);
#3792=AXIS2_PLACEMENT_3D('',#8079,#4737,#4738);
#3793=AXIS2_PLACEMENT_3D('',#8083,#4740,#4741);
#3794=AXIS2_PLACEMENT_3D('',#8085,#4743,#4744);
#3795=AXIS2_PLACEMENT_3D('',#8090,#4746,#4747);
#3796=AXIS2_PLACEMENT_3D('',#8095,#4750,#4751);
#3797=AXIS2_PLACEMENT_3D('',#8099,#4753,#4754);
#3798=AXIS2_PLACEMENT_3D('',#8103,#4756,#4757);
#3799=AXIS2_PLACEMENT_3D('',#8106,#4759,#4760);
#3800=AXIS2_PLACEMENT_3D('',#8107,#4761,#4762);
#3801=AXIS2_PLACEMENT_3D('',#8109,#4763,#4764);
#3802=AXIS2_PLACEMENT_3D('',#8110,#4765,#4766);
#3803=AXIS2_PLACEMENT_3D('',#8111,#4767,#4768);
#3804=AXIS2_PLACEMENT_3D('',#8114,#4769,#4770);
#3805=AXIS2_PLACEMENT_3D('',#8116,#4771,#4772);
#3806=AXIS2_PLACEMENT_3D('',#8117,#4773,#4774);
#3807=AXIS2_PLACEMENT_3D('',#8118,#4775,#4776);
#3808=AXIS2_PLACEMENT_3D('',#8121,#4777,#4778);
#3809=AXIS2_PLACEMENT_3D('',#8123,#4779,#4780);
#3810=AXIS2_PLACEMENT_3D('',#8124,#4781,#4782);
#3811=AXIS2_PLACEMENT_3D('',#8125,#4783,#4784);
#3812=AXIS2_PLACEMENT_3D('',#8128,#4785,#4786);
#3813=AXIS2_PLACEMENT_3D('',#8154,#4787,#4788);
#3814=AXIS2_PLACEMENT_3D('',#8155,#4789,#4790);
#3815=AXIS2_PLACEMENT_3D('',#8157,#4791,#4792);
#3816=AXIS2_PLACEMENT_3D('',#8158,#4793,#4794);
#3817=AXIS2_PLACEMENT_3D('',#8159,#4795,#4796);
#3818=AXIS2_PLACEMENT_3D('',#8162,#4797,#4798);
#3819=AXIS2_PLACEMENT_3D('',#8164,#4799,#4800);
#3820=AXIS2_PLACEMENT_3D('',#8165,#4801,#4802);
#3821=AXIS2_PLACEMENT_3D('',#8166,#4803,#4804);
#3822=AXIS2_PLACEMENT_3D('',#8169,#4805,#4806);
#3823=AXIS2_PLACEMENT_3D('',#8171,#4807,#4808);
#3824=AXIS2_PLACEMENT_3D('',#8172,#4809,#4810);
#3825=AXIS2_PLACEMENT_3D('',#8173,#4811,#4812);
#3826=AXIS2_PLACEMENT_3D('',#8176,#4813,#4814);
#3827=AXIS2_PLACEMENT_3D('',#8178,#4815,#4816);
#3828=AXIS2_PLACEMENT_3D('',#8179,#4817,#4818);
#3829=AXIS2_PLACEMENT_3D('',#8180,#4819,#4820);
#3830=AXIS2_PLACEMENT_3D('',#8181,#4821,#4822);
#3831=AXIS2_PLACEMENT_3D('',#8182,#4823,#4824);
#3832=AXIS2_PLACEMENT_3D('',#8183,#4825,#4826);
#3833=AXIS2_PLACEMENT_3D('',#8184,#4827,#4828);
#3834=AXIS2_PLACEMENT_3D('',#8185,#4829,#4830);
#3835=AXIS2_PLACEMENT_3D('',#8186,#4831,#4832);
#3836=AXIS2_PLACEMENT_3D('',#8187,#4833,#4834);
#3837=AXIS2_PLACEMENT_3D('',#8188,#4835,#4836);
#3838=AXIS2_PLACEMENT_3D('',#8189,#4837,#4838);
#3839=AXIS2_PLACEMENT_3D('',#8190,#4839,#4840);
#3840=AXIS2_PLACEMENT_3D('',#8191,#4841,#4842);
#3841=AXIS2_PLACEMENT_3D('',#8192,#4843,#4844);
#3842=AXIS2_PLACEMENT_3D('',#8193,#4845,#4846);
#3843=AXIS2_PLACEMENT_3D('',#8194,#4847,#4848);
#3844=AXIS2_PLACEMENT_3D('',#8195,#4849,#4850);
#3845=AXIS2_PLACEMENT_3D('',#8196,#4851,#4852);
#3846=AXIS2_PLACEMENT_3D('',#8197,#4853,#4854);
#3847=AXIS2_PLACEMENT_3D('',#8198,#4855,#4856);
#3848=AXIS2_PLACEMENT_3D('',#8199,#4857,#4858);
#3849=AXIS2_PLACEMENT_3D('',#8200,#4859,#4860);
#3850=AXIS2_PLACEMENT_3D('',#8201,#4861,#4862);
#3851=AXIS2_PLACEMENT_3D('',#8202,#4863,#4864);
#3852=AXIS2_PLACEMENT_3D('',#8203,#4865,#4866);
#3853=AXIS2_PLACEMENT_3D('',#8204,#4867,#4868);
#3854=AXIS2_PLACEMENT_3D('',#8205,#4869,#4870);
#3855=AXIS2_PLACEMENT_3D('',#8206,#4871,#4872);
#3856=AXIS2_PLACEMENT_3D('',#8207,#4873,#4874);
#3857=AXIS2_PLACEMENT_3D('',#8208,#4875,#4876);
#3858=AXIS2_PLACEMENT_3D('',#8209,#4877,#4878);
#3859=AXIS2_PLACEMENT_3D('',#8210,#4879,#4880);
#3860=AXIS2_PLACEMENT_3D('',#8211,#4881,#4882);
#3861=AXIS2_PLACEMENT_3D('',#8212,#4883,#4884);
#3862=AXIS2_PLACEMENT_3D('',#8213,#4885,#4886);
#3863=AXIS2_PLACEMENT_3D('',#8214,#4887,#4888);
#3864=AXIS2_PLACEMENT_3D('',#8215,#4889,#4890);
#3865=AXIS2_PLACEMENT_3D('',#8216,#4891,#4892);
#3866=AXIS2_PLACEMENT_3D('',#8217,#4893,#4894);
#3867=AXIS2_PLACEMENT_3D('',#8218,#4895,#4896);
#3868=AXIS2_PLACEMENT_3D('',#8219,#4897,#4898);
#3869=AXIS2_PLACEMENT_3D('',#8220,#4899,#4900);
#3870=AXIS2_PLACEMENT_3D('',#8221,#4901,#4902);
#3871=AXIS2_PLACEMENT_3D('',#8222,#4903,#4904);
#3872=AXIS2_PLACEMENT_3D('',#8223,#4905,#4906);
#3873=AXIS2_PLACEMENT_3D('',#8224,#4907,#4908);
#3874=AXIS2_PLACEMENT_3D('',#8225,#4909,#4910);
#3875=AXIS2_PLACEMENT_3D('',#8226,#4911,#4912);
#3876=AXIS2_PLACEMENT_3D('',#8227,#4913,#4914);
#3877=AXIS2_PLACEMENT_3D('',#8228,#4915,#4916);
#3878=AXIS2_PLACEMENT_3D('',#8229,#4917,#4918);
#3879=AXIS2_PLACEMENT_3D('',#8230,#4919,#4920);
#3880=AXIS2_PLACEMENT_3D('',#8231,#4921,#4922);
#3881=AXIS2_PLACEMENT_3D('',#8232,#4923,#4924);
#3882=AXIS2_PLACEMENT_3D('',#8233,#4925,#4926);
#3883=AXIS2_PLACEMENT_3D('',#8234,#4927,#4928);
#3884=AXIS2_PLACEMENT_3D('',#8235,#4929,#4930);
#3885=AXIS2_PLACEMENT_3D('',#8236,#4931,#4932);
#3886=AXIS2_PLACEMENT_3D('',#8237,#4933,#4934);
#3887=AXIS2_PLACEMENT_3D('',#8238,#4935,#4936);
#3888=AXIS2_PLACEMENT_3D('',#8239,#4937,#4938);
#3889=AXIS2_PLACEMENT_3D('',#8240,#4939,#4940);
#3890=AXIS2_PLACEMENT_3D('',#8241,#4941,#4942);
#3891=AXIS2_PLACEMENT_3D('',#8242,#4943,#4944);
#3892=AXIS2_PLACEMENT_3D('',#8243,#4945,#4946);
#3893=AXIS2_PLACEMENT_3D('',#8244,#4947,#4948);
#3894=AXIS2_PLACEMENT_3D('',#8245,#4949,#4950);
#3895=AXIS2_PLACEMENT_3D('',#8246,#4951,#4952);
#3896=AXIS2_PLACEMENT_3D('',#8247,#4953,#4954);
#3897=AXIS2_PLACEMENT_3D('',#8248,#4955,#4956);
#3898=AXIS2_PLACEMENT_3D('',#8249,#4957,#4958);
#3899=AXIS2_PLACEMENT_3D('',#8250,#4959,#4960);
#3900=AXIS2_PLACEMENT_3D('',#8251,#4961,#4962);
#3901=AXIS2_PLACEMENT_3D('',#8252,#4963,#4964);
#3902=AXIS2_PLACEMENT_3D('',#8253,#4965,#4966);
#3903=AXIS2_PLACEMENT_3D('',#8254,#4967,#4968);
#3904=AXIS2_PLACEMENT_3D('',#8255,#4969,#4970);
#3905=AXIS2_PLACEMENT_3D('',#8256,#4971,#4972);
#3906=AXIS2_PLACEMENT_3D('',#8257,#4973,#4974);
#3907=AXIS2_PLACEMENT_3D('',#8258,#4975,#4976);
#3908=AXIS2_PLACEMENT_3D('',#8259,#4977,#4978);
#3909=AXIS2_PLACEMENT_3D('',#8260,#4979,#4980);
#3910=AXIS2_PLACEMENT_3D('',#8261,#4981,#4982);
#3911=AXIS2_PLACEMENT_3D('',#8262,#4983,#4984);
#3912=AXIS2_PLACEMENT_3D('',#8263,#4985,#4986);
#3913=AXIS2_PLACEMENT_3D('',#8264,#4987,#4988);
#3914=AXIS2_PLACEMENT_3D('',#8265,#4989,#4990);
#3915=AXIS2_PLACEMENT_3D('',#8266,#4991,#4992);
#3916=AXIS2_PLACEMENT_3D('',#8267,#4993,#4994);
#3917=AXIS2_PLACEMENT_3D('',#8268,#4995,#4996);
#3918=AXIS2_PLACEMENT_3D('',#8269,#4997,#4998);
#3919=AXIS2_PLACEMENT_3D('',#8270,#4999,#5000);
#3920=AXIS2_PLACEMENT_3D('',#8271,#5001,#5002);
#3921=AXIS2_PLACEMENT_3D('',#8272,#5003,#5004);
#3922=AXIS2_PLACEMENT_3D('',#8273,#5005,#5006);
#3923=AXIS2_PLACEMENT_3D('',#8274,#5007,#5008);
#3924=AXIS2_PLACEMENT_3D('',#8275,#5009,#5010);
#3925=AXIS2_PLACEMENT_3D('',#8276,#5011,#5012);
#3926=AXIS2_PLACEMENT_3D('',#8277,#5013,#5014);
#3927=AXIS2_PLACEMENT_3D('',#8278,#5015,#5016);
#3928=AXIS2_PLACEMENT_3D('',#8279,#5017,#5018);
#3929=AXIS2_PLACEMENT_3D('',#8280,#5019,#5020);
#3930=AXIS2_PLACEMENT_3D('',#8281,#5021,#5022);
#3931=AXIS2_PLACEMENT_3D('',#8282,#5023,#5024);
#3932=AXIS2_PLACEMENT_3D('',#8283,#5025,#5026);
#3933=AXIS2_PLACEMENT_3D('',#8284,#5027,#5028);
#3934=AXIS2_PLACEMENT_3D('',#8285,#5029,#5030);
#3935=AXIS2_PLACEMENT_3D('',#8286,#5031,#5032);
#3936=AXIS2_PLACEMENT_3D('',#8287,#5033,#5034);
#3937=AXIS2_PLACEMENT_3D('',#8288,#5035,#5036);
#3938=AXIS2_PLACEMENT_3D('',#8289,#5037,#5038);
#3939=AXIS2_PLACEMENT_3D('',#8290,#5039,#5040);
#3940=AXIS2_PLACEMENT_3D('',#8291,#5041,#5042);
#3941=AXIS2_PLACEMENT_3D('',#8292,#5043,#5044);
#3942=AXIS2_PLACEMENT_3D('',#8293,#5045,#5046);
#3943=AXIS2_PLACEMENT_3D('',#8294,#5047,#5048);
#3944=AXIS2_PLACEMENT_3D('',#8295,#5049,#5050);
#3945=AXIS2_PLACEMENT_3D('',#8296,#5051,#5052);
#3946=AXIS2_PLACEMENT_3D('',#8297,#5053,#5054);
#3947=AXIS2_PLACEMENT_3D('',#8298,#5055,#5056);
#3948=AXIS2_PLACEMENT_3D('',#8299,#5057,#5058);
#3949=AXIS2_PLACEMENT_3D('',#8300,#5059,#5060);
#3950=AXIS2_PLACEMENT_3D('',#8301,#5061,#5062);
#3951=AXIS2_PLACEMENT_3D('',#8302,#5063,#5064);
#3952=AXIS2_PLACEMENT_3D('',#8303,#5065,#5066);
#3953=AXIS2_PLACEMENT_3D('',#8304,#5067,#5068);
#3954=AXIS2_PLACEMENT_3D('',#8305,#5069,#5070);
#3955=AXIS2_PLACEMENT_3D('',#8306,#5071,#5072);
#3956=AXIS2_PLACEMENT_3D('',#8307,#5073,#5074);
#3957=AXIS2_PLACEMENT_3D('',#8308,#5075,#5076);
#3958=AXIS2_PLACEMENT_3D('',#8309,#5077,#5078);
#3959=AXIS2_PLACEMENT_3D('',#8310,#5079,#5080);
#3960=AXIS2_PLACEMENT_3D('',#8311,#5081,#5082);
#3961=AXIS2_PLACEMENT_3D('',#8312,#5083,#5084);
#3962=AXIS2_PLACEMENT_3D('',#8313,#5085,#5086);
#3963=AXIS2_PLACEMENT_3D('',#8314,#5087,#5088);
#3964=AXIS2_PLACEMENT_3D('',#8315,#5089,#5090);
#3965=AXIS2_PLACEMENT_3D('',#8316,#5091,#5092);
#3966=AXIS2_PLACEMENT_3D('',#8317,#5093,#5094);
#3967=AXIS2_PLACEMENT_3D('',#8318,#5095,#5096);
#3968=AXIS2_PLACEMENT_3D('',#8319,#5097,#5098);
#3969=AXIS2_PLACEMENT_3D('',#8320,#5099,#5100);
#3970=AXIS2_PLACEMENT_3D('',#8321,#5101,#5102);
#3971=AXIS2_PLACEMENT_3D('',#8322,#5103,#5104);
#3972=AXIS2_PLACEMENT_3D('',#8323,#5105,#5106);
#3973=AXIS2_PLACEMENT_3D('',#8324,#5107,#5108);
#3974=AXIS2_PLACEMENT_3D('',#8325,#5109,#5110);
#3975=AXIS2_PLACEMENT_3D('',#8326,#5111,#5112);
#3976=AXIS2_PLACEMENT_3D('',#8327,#5113,#5114);
#3977=AXIS2_PLACEMENT_3D('',#8328,#5115,#5116);
#3978=AXIS2_PLACEMENT_3D('',#8329,#5117,#5118);
#3979=AXIS2_PLACEMENT_3D('',#8330,#5119,#5120);
#3980=AXIS2_PLACEMENT_3D('',#8331,#5121,#5122);
#3981=AXIS2_PLACEMENT_3D('',#8332,#5123,#5124);
#3982=AXIS2_PLACEMENT_3D('',#8333,#5125,#5126);
#3983=AXIS2_PLACEMENT_3D('',#8334,#5127,#5128);
#3984=AXIS2_PLACEMENT_3D('',#8335,#5129,#5130);
#3985=AXIS2_PLACEMENT_3D('',#8336,#5131,#5132);
#3986=AXIS2_PLACEMENT_3D('',#8337,#5133,#5134);
#3987=AXIS2_PLACEMENT_3D('',#8338,#5135,#5136);
#3988=AXIS2_PLACEMENT_3D('',#8339,#5137,#5138);
#3989=AXIS2_PLACEMENT_3D('',#8340,#5139,#5140);
#3990=AXIS2_PLACEMENT_3D('',#8341,#5141,#5142);
#3991=AXIS2_PLACEMENT_3D('',#8342,#5143,#5144);
#3992=AXIS2_PLACEMENT_3D('',#8343,#5145,#5146);
#3993=AXIS2_PLACEMENT_3D('',#8344,#5147,#5148);
#3994=AXIS2_PLACEMENT_3D('',#8345,#5149,#5150);
#3995=AXIS2_PLACEMENT_3D('',#8346,#5151,#5152);
#3996=AXIS2_PLACEMENT_3D('',#8347,#5153,#5154);
#3997=AXIS2_PLACEMENT_3D('',#8348,#5155,#5156);
#3998=AXIS2_PLACEMENT_3D('',#8349,#5157,#5158);
#3999=AXIS2_PLACEMENT_3D('',#8350,#5159,#5160);
#4000=AXIS2_PLACEMENT_3D('',#8351,#5161,#5162);
#4001=AXIS2_PLACEMENT_3D('',#8352,#5163,#5164);
#4002=AXIS2_PLACEMENT_3D('',#8353,#5165,#5166);
#4003=AXIS2_PLACEMENT_3D('',#8354,#5167,#5168);
#4004=AXIS2_PLACEMENT_3D('',#8355,#5169,#5170);
#4005=AXIS2_PLACEMENT_3D('',#8356,#5171,#5172);
#4006=AXIS2_PLACEMENT_3D('',#8357,#5173,#5174);
#4007=AXIS2_PLACEMENT_3D('',#8358,#5175,#5176);
#4008=AXIS2_PLACEMENT_3D('',#8359,#5177,#5178);
#4009=AXIS2_PLACEMENT_3D('',#8360,#5179,#5180);
#4010=AXIS2_PLACEMENT_3D('',#8361,#5181,#5182);
#4011=AXIS2_PLACEMENT_3D('',#8362,#5183,#5184);
#4012=AXIS2_PLACEMENT_3D('',#8363,#5185,#5186);
#4013=AXIS2_PLACEMENT_3D('',#8364,#5187,#5188);
#4014=AXIS2_PLACEMENT_3D('',#8366,#5189,#5190);
#4015=AXIS2_PLACEMENT_3D('',#8367,#5191,#5192);
#4016=AXIS2_PLACEMENT_3D('',#8368,#5193,#5194);
#4017=AXIS2_PLACEMENT_3D('',#8369,#5195,#5196);
#4018=AXIS2_PLACEMENT_3D('',#8371,#5197,#5198);
#4019=AXIS2_PLACEMENT_3D('',#8372,#5199,#5200);
#4020=AXIS2_PLACEMENT_3D('',#8373,#5201,#5202);
#4021=AXIS2_PLACEMENT_3D('',#8375,#5203,#5204);
#4022=AXIS2_PLACEMENT_3D('',#8376,#5205,#5206);
#4023=AXIS2_PLACEMENT_3D('',#8435,#5207,#5208);
#4024=AXIS2_PLACEMENT_3D('',#9478,#5209,#5210);
#4025=AXIS2_PLACEMENT_3D('',#10519,#5211,#5212);
#4026=AXIS2_PLACEMENT_3D('',#10520,#5213,#5214);
#4027=AXIS2_PLACEMENT_3D('',#10521,#5215,#5216);
#4028=AXIS2_PLACEMENT_3D('',#10522,#5217,#5218);
#4029=AXIS2_PLACEMENT_3D('',#10523,#5219,#5220);
#4030=AXIS2_PLACEMENT_3D('',#10524,#5221,#5222);
#4031=AXIS2_PLACEMENT_3D('',#10525,#5223,#5224);
#4032=AXIS2_PLACEMENT_3D('',#10526,#5225,#5226);
#4033=AXIS2_PLACEMENT_3D('',#10527,#5227,#5228);
#4034=AXIS2_PLACEMENT_3D('',#10528,#5229,#5230);
#4035=AXIS2_PLACEMENT_3D('',#10529,#5231,#5232);
#4036=DIRECTION('axis',(0.,0.,1.));
#4037=DIRECTION('refdir',(1.,0.,0.));
#4038=DIRECTION('axis',(0.,0.,1.));
#4039=DIRECTION('refdir',(1.,0.,0.));
#4040=DIRECTION('center_axis',(0.,0.,1.));
#4041=DIRECTION('ref_axis',(1.,0.,0.));
#4042=DIRECTION('center_axis',(-3.61400724161835E-16,0.,-1.));
#4043=DIRECTION('ref_axis',(1.,0.,-3.61400724161835E-16));
#4044=DIRECTION('',(0.,0.,1.));
#4045=DIRECTION('center_axis',(0.,0.,1.));
#4046=DIRECTION('ref_axis',(1.,0.,0.));
#4047=DIRECTION('center_axis',(0.,0.,1.));
#4048=DIRECTION('ref_axis',(1.,0.,0.));
#4049=DIRECTION('center_axis',(-3.61400724161835E-16,0.,-1.));
#4050=DIRECTION('ref_axis',(1.,0.,-3.61400724161835E-16));
#4051=DIRECTION('',(0.,0.,1.));
#4052=DIRECTION('center_axis',(0.,0.,1.));
#4053=DIRECTION('ref_axis',(1.,0.,0.));
#4054=DIRECTION('center_axis',(1.,0.,-2.23835287222814E-16));
#4055=DIRECTION('ref_axis',(-2.23835287222814E-16,0.,-1.));
#4056=DIRECTION('center_axis',(-1.,0.,1.32421639387543E-16));
#4057=DIRECTION('ref_axis',(-1.32421639387543E-16,0.,-1.));
#4058=DIRECTION('',(1.,0.,-2.23835287222814E-16));
#4059=DIRECTION('center_axis',(1.,0.,-2.23835287222814E-16));
#4060=DIRECTION('ref_axis',(-2.23835287222814E-16,0.,-1.));
#4061=DIRECTION('center_axis',(1.,0.,-3.35752930834221E-16));
#4062=DIRECTION('ref_axis',(-3.35752930834221E-16,0.,-1.));
#4063=DIRECTION('',(0.,-1.,0.));
#4064=DIRECTION('',(0.,0.,1.));
#4065=DIRECTION('',(0.,1.,0.));
#4066=DIRECTION('',(3.35752930834221E-16,0.,1.));
#4067=DIRECTION('center_axis',(1.,0.,-3.35752930834221E-16));
#4068=DIRECTION('ref_axis',(-3.35752930834221E-16,0.,-1.));
#4069=DIRECTION('',(0.,1.,0.));
#4070=DIRECTION('',(0.,0.,1.));
#4071=DIRECTION('',(0.,-1.,0.));
#4072=DIRECTION('',(3.35752930834221E-16,0.,1.));
#4073=DIRECTION('center_axis',(1.,0.,-3.35752930834221E-16));
#4074=DIRECTION('ref_axis',(-3.35752930834221E-16,0.,-1.));
#4075=DIRECTION('',(0.,1.,0.));
#4076=DIRECTION('',(0.,0.,1.));
#4077=DIRECTION('',(0.,-1.,0.));
#4078=DIRECTION('',(3.35752930834221E-16,0.,1.));
#4079=DIRECTION('center_axis',(1.,0.,-3.35752930834221E-16));
#4080=DIRECTION('ref_axis',(-3.35752930834221E-16,0.,-1.));
#4081=DIRECTION('',(0.,-1.,0.));
#4082=DIRECTION('',(0.,0.,1.));
#4083=DIRECTION('',(0.,1.,0.));
#4084=DIRECTION('',(3.35752930834221E-16,0.,1.));
#4085=DIRECTION('center_axis',(0.,0.,-1.));
#4086=DIRECTION('ref_axis',(-1.,0.,0.));
#4087=DIRECTION('',(-1.,-4.33680868994202E-16,0.));
#4088=DIRECTION('',(-3.1256278846429E-16,1.,0.));
#4089=DIRECTION('',(1.,0.,0.));
#4090=DIRECTION('',(1.,0.,0.));
#4091=DIRECTION('',(0.,1.,0.));
#4092=DIRECTION('',(1.,0.,0.));
#4093=DIRECTION('center_axis',(-1.,0.,2.23835287222814E-16));
#4094=DIRECTION('ref_axis',(2.23835287222814E-16,0.,1.));
#4095=DIRECTION('',(-2.23835287222814E-16,0.,-1.));
#4096=DIRECTION('',(0.,-1.,0.));
#4097=DIRECTION('',(-2.23835287222814E-16,0.,-1.));
#4098=DIRECTION('',(0.,1.,0.));
#4099=DIRECTION('center_axis',(0.,0.,1.));
#4100=DIRECTION('ref_axis',(1.,0.,0.));
#4101=DIRECTION('',(-3.1256278846429E-16,1.,0.));
#4102=DIRECTION('',(-1.,-4.33680868994202E-16,0.));
#4103=DIRECTION('',(-1.,0.,0.));
#4104=DIRECTION('',(0.,-1.,0.));
#4105=DIRECTION('',(-1.,0.,0.));
#4106=DIRECTION('',(1.,0.,0.));
#4107=DIRECTION('center_axis',(0.,1.,0.));
#4108=DIRECTION('ref_axis',(0.,0.,1.));
#4109=DIRECTION('center_axis',(0.,1.,0.));
#4110=DIRECTION('ref_axis',(0.,0.,1.));
#4111=DIRECTION('center_axis',(0.,1.,0.));
#4112=DIRECTION('ref_axis',(0.,0.,1.));
#4113=DIRECTION('',(-1.,0.,0.));
#4114=DIRECTION('center_axis',(0.,-1.,0.));
#4115=DIRECTION('ref_axis',(0.,0.,1.));
#4116=DIRECTION('',(-1.32421639387543E-16,0.,-1.));
#4117=DIRECTION('center_axis',(0.,-1.,0.));
#4118=DIRECTION('ref_axis',(2.60208521396522E-14,0.,1.));
#4119=DIRECTION('',(1.,0.,-3.61400724161835E-16));
#4120=DIRECTION('center_axis',(0.,1.,0.));
#4121=DIRECTION('ref_axis',(0.,0.,1.));
#4122=DIRECTION('center_axis',(0.,-1.,0.));
#4123=DIRECTION('ref_axis',(5.20417042793042E-15,0.,1.));
#4124=DIRECTION('',(1.,0.,-3.61400724161835E-16));
#4125=DIRECTION('center_axis',(0.,1.,0.));
#4126=DIRECTION('ref_axis',(0.,0.,1.));
#4127=DIRECTION('',(-1.32421639387543E-16,0.,-1.));
#4128=DIRECTION('center_axis',(0.,1.,0.));
#4129=DIRECTION('ref_axis',(0.,0.,1.));
#4130=DIRECTION('',(-1.,0.,0.));
#4131=DIRECTION('center_axis',(0.,-1.,0.));
#4132=DIRECTION('ref_axis',(0.,0.,1.));
#4133=DIRECTION('center_axis',(0.,0.,-1.));
#4134=DIRECTION('ref_axis',(-1.,0.,0.));
#4135=DIRECTION('',(1.,4.33680868994202E-16,0.));
#4136=DIRECTION('',(3.1256278846429E-16,-1.,0.));
#4137=DIRECTION('',(-1.,0.,0.));
#4138=DIRECTION('',(0.,1.,0.));
#4139=DIRECTION('center_axis',(1.,0.,-1.32421639387543E-16));
#4140=DIRECTION('ref_axis',(-1.32421639387543E-16,0.,-1.));
#4141=DIRECTION('',(0.,1.,0.));
#4142=DIRECTION('',(0.,-1.,0.));
#4143=DIRECTION('center_axis',(3.61400724161835E-16,0.,1.));
#4144=DIRECTION('ref_axis',(1.,0.,-3.61400724161835E-16));
#4145=DIRECTION('',(-3.1256278846429E-16,1.,1.12960418097037E-31));
#4146=DIRECTION('',(-1.,-4.33680868994202E-16,3.61400724161835E-16));
#4147=DIRECTION('',(0.,-1.,0.));
#4148=DIRECTION('',(1.,0.,-3.61400724161835E-16));
#4149=DIRECTION('center_axis',(0.,-1.,0.));
#4150=DIRECTION('ref_axis',(0.,0.,-1.));
#4151=DIRECTION('center_axis',(0.,-1.,0.));
#4152=DIRECTION('ref_axis',(0.,0.,-1.));
#4153=DIRECTION('center_axis',(0.,-1.,0.));
#4154=DIRECTION('ref_axis',(0.,0.,-1.));
#4155=DIRECTION('center_axis',(0.,-1.,0.));
#4156=DIRECTION('ref_axis',(0.,0.,-1.));
#4157=DIRECTION('center_axis',(0.,-1.,0.));
#4158=DIRECTION('ref_axis',(0.,0.,-1.));
#4159=DIRECTION('',(0.,0.,1.));
#4160=DIRECTION('center_axis',(1.,3.1256278846429E-16,0.));
#4161=DIRECTION('ref_axis',(-3.1256278846429E-16,1.,0.));
#4162=DIRECTION('',(0.,0.,1.));
#4163=DIRECTION('center_axis',(-4.33680868994202E-16,1.,0.));
#4164=DIRECTION('ref_axis',(-1.,-4.33680868994202E-16,0.));
#4165=DIRECTION('center_axis',(-4.33680868994202E-16,1.,0.));
#4166=DIRECTION('ref_axis',(-1.,-4.33680868994202E-16,0.));
#4167=DIRECTION('',(0.,0.,1.));
#4168=DIRECTION('center_axis',(1.,3.1256278846429E-16,0.));
#4169=DIRECTION('ref_axis',(-3.1256278846429E-16,1.,0.));
#4170=DIRECTION('',(0.,0.,1.));
#4171=DIRECTION('center_axis',(0.,-1.,0.));
#4172=DIRECTION('ref_axis',(0.,0.,-1.));
#4173=DIRECTION('axis',(0.,0.,1.));
#4174=DIRECTION('refdir',(1.,0.,0.));
#4175=DIRECTION('center_axis',(1.,1.85863229568944E-16,0.));
#4176=DIRECTION('ref_axis',(-1.85863229568944E-16,1.,0.));
#4177=DIRECTION('center_axis',(-1.,-1.85863229568944E-16,0.));
#4178=DIRECTION('ref_axis',(-1.85863229568944E-16,1.,0.));
#4179=DIRECTION('',(1.,1.85863229568944E-16,0.));
#4180=DIRECTION('center_axis',(1.,1.85863229568944E-16,0.));
#4181=DIRECTION('ref_axis',(-1.85863229568944E-16,1.,0.));
#4182=DIRECTION('center_axis',(-1.,-1.85863229568944E-16,0.));
#4183=DIRECTION('ref_axis',(1.85863229568944E-16,-1.,0.));
#4184=DIRECTION('center_axis',(1.,2.66880534765663E-16,0.));
#4185=DIRECTION('ref_axis',(-2.66880534765663E-16,1.,0.));
#4186=DIRECTION('',(1.,1.85863229568944E-16,0.));
#4187=DIRECTION('center_axis',(1.,2.66880534765663E-16,0.));
#4188=DIRECTION('ref_axis',(-2.66880534765663E-16,1.,0.));
#4189=DIRECTION('center_axis',(-1.,-1.85863229568944E-16,0.));
#4190=DIRECTION('ref_axis',(1.85863229568944E-16,-1.,0.));
#4191=DIRECTION('center_axis',(1.,2.66880534765663E-16,0.));
#4192=DIRECTION('ref_axis',(-2.66880534765663E-16,1.,0.));
#4193=DIRECTION('',(1.,1.85863229568944E-16,0.));
#4194=DIRECTION('center_axis',(-1.,-1.85863229568944E-16,0.));
#4195=DIRECTION('ref_axis',(1.85863229568944E-16,-1.,0.));
#4196=DIRECTION('center_axis',(-1.,-1.85863229568944E-16,0.));
#4197=DIRECTION('ref_axis',(1.85863229568944E-16,-1.,0.));
#4198=DIRECTION('center_axis',(-2.48016390503164E-32,1.33440267382831E-16,
-1.));
#4199=DIRECTION('ref_axis',(0.,1.,1.33440267382831E-16));
#4200=DIRECTION('',(2.66880534765663E-16,-1.,-1.33440267382831E-16));
#4201=DIRECTION('',(1.,1.85863229568944E-16,5.47382212626882E-48));
#4202=DIRECTION('',(2.66880534765663E-16,-1.,-1.33440267382831E-16));
#4203=DIRECTION('',(-1.,-1.85863229568944E-16,-5.47382212626882E-48));
#4204=DIRECTION('center_axis',(-1.85863229568944E-16,1.,0.));
#4205=DIRECTION('ref_axis',(-1.,-1.85863229568944E-16,0.));
#4206=DIRECTION('',(0.,0.,-1.));
#4207=DIRECTION('',(1.,1.85863229568944E-16,5.47382212626882E-48));
#4208=DIRECTION('',(0.,0.,-1.));
#4209=DIRECTION('',(-1.,-1.85863229568944E-16,-5.47382212626882E-48));
#4210=DIRECTION('center_axis',(2.48016390503164E-32,-1.33440267382831E-16,
1.));
#4211=DIRECTION('ref_axis',(0.,-1.,-1.33440267382831E-16));
#4212=DIRECTION('',(-2.66880534765663E-16,1.,1.33440267382831E-16));
#4213=DIRECTION('',(-1.,-1.85863229568944E-16,-5.47382212626882E-48));
#4214=DIRECTION('',(-2.66880534765663E-16,1.,1.33440267382831E-16));
#4215=DIRECTION('',(1.,1.85863229568944E-16,5.47382212626882E-48));
#4216=DIRECTION('center_axis',(1.85863229568944E-16,-1.,0.));
#4217=DIRECTION('ref_axis',(1.,1.85863229568944E-16,0.));
#4218=DIRECTION('',(0.,0.,1.));
#4219=DIRECTION('',(-1.,-1.85863229568944E-16,-5.47382212626882E-48));
#4220=DIRECTION('',(0.,0.,1.));
#4221=DIRECTION('',(1.,1.85863229568944E-16,5.47382212626882E-48));
#4222=DIRECTION('center_axis',(1.,2.66880534765663E-16,0.));
#4223=DIRECTION('ref_axis',(-2.66880534765663E-16,1.,0.));
#4224=DIRECTION('center_axis',(1.,2.66880534765663E-16,0.));
#4225=DIRECTION('ref_axis',(-2.66880534765663E-16,1.,0.));
#4226=DIRECTION('center_axis',(1.,2.66880534765663E-16,0.));
#4227=DIRECTION('ref_axis',(-2.66880534765663E-16,1.,0.));
#4228=DIRECTION('center_axis',(1.,2.66880534765663E-16,0.));
#4229=DIRECTION('ref_axis',(-2.66880534765663E-16,1.,0.));
#4230=DIRECTION('center_axis',(1.,2.66880534765663E-16,0.));
#4231=DIRECTION('ref_axis',(-2.66880534765663E-16,1.,0.));
#4232=DIRECTION('center_axis',(1.,2.66880534765663E-16,0.));
#4233=DIRECTION('ref_axis',(-2.66880534765663E-16,1.,0.));
#4234=DIRECTION('center_axis',(-1.,-2.66880534765663E-16,0.));
#4235=DIRECTION('ref_axis',(-2.66880534765663E-16,1.,0.));
#4236=DIRECTION('center_axis',(-1.,-2.66880534765663E-16,0.));
#4237=DIRECTION('ref_axis',(-2.66880534765663E-16,1.,0.));
#4238=DIRECTION('center_axis',(-1.,-2.66880534765663E-16,0.));
#4239=DIRECTION('ref_axis',(-2.66880534765663E-16,1.,0.));
#4240=DIRECTION('center_axis',(-1.,-2.66880534765663E-16,0.));
#4241=DIRECTION('ref_axis',(-2.66880534765663E-16,1.,0.));
#4242=DIRECTION('center_axis',(-2.48016390503164E-32,1.33440267382831E-16,
-1.));
#4243=DIRECTION('ref_axis',(0.,1.,1.33440267382831E-16));
#4244=DIRECTION('',(2.66880534765663E-16,-1.,-1.33440267382831E-16));
#4245=DIRECTION('',(-1.,-1.85863229568944E-16,-5.47382212626882E-48));
#4246=DIRECTION('',(2.66880534765663E-16,-1.,-1.33440267382831E-16));
#4247=DIRECTION('',(1.,1.85863229568944E-16,5.47382212626882E-48));
#4248=DIRECTION('center_axis',(-1.85863229568944E-16,1.,0.));
#4249=DIRECTION('ref_axis',(-1.,-1.85863229568944E-16,0.));
#4250=DIRECTION('',(0.,0.,-1.));
#4251=DIRECTION('',(-1.,-1.85863229568944E-16,-5.47382212626882E-48));
#4252=DIRECTION('',(0.,0.,-1.));
#4253=DIRECTION('',(1.,1.85863229568944E-16,5.47382212626882E-48));
#4254=DIRECTION('center_axis',(2.48016390503164E-32,-1.33440267382831E-16,
1.));
#4255=DIRECTION('ref_axis',(0.,-1.,-1.33440267382831E-16));
#4256=DIRECTION('',(-2.66880534765663E-16,1.,1.33440267382831E-16));
#4257=DIRECTION('',(1.,1.85863229568944E-16,5.47382212626882E-48));
#4258=DIRECTION('',(-2.66880534765663E-16,1.,1.33440267382831E-16));
#4259=DIRECTION('',(-1.,-1.85863229568944E-16,-5.47382212626882E-48));
#4260=DIRECTION('center_axis',(1.85863229568944E-16,-1.,0.));
#4261=DIRECTION('ref_axis',(1.,1.85863229568944E-16,0.));
#4262=DIRECTION('',(0.,0.,1.));
#4263=DIRECTION('',(1.,1.85863229568944E-16,5.47382212626882E-48));
#4264=DIRECTION('',(0.,0.,1.));
#4265=DIRECTION('',(-1.,-1.85863229568944E-16,-5.47382212626882E-48));
#4266=DIRECTION('center_axis',(1.,2.66880534765663E-16,0.));
#4267=DIRECTION('ref_axis',(-2.66880534765663E-16,1.,0.));
#4268=DIRECTION('center_axis',(1.,2.66880534765663E-16,0.));
#4269=DIRECTION('ref_axis',(-2.66880534765663E-16,1.,0.));
#4270=DIRECTION('center_axis',(1.,2.66880534765663E-16,0.));
#4271=DIRECTION('ref_axis',(-2.66880534765663E-16,1.,0.));
#4272=DIRECTION('center_axis',(1.,2.66880534765663E-16,0.));
#4273=DIRECTION('ref_axis',(-2.66880534765663E-16,1.,0.));
#4274=DIRECTION('center_axis',(1.,2.66880534765663E-16,0.));
#4275=DIRECTION('ref_axis',(-2.66880534765663E-16,1.,0.));
#4276=DIRECTION('center_axis',(1.,1.85863229568944E-16,0.));
#4277=DIRECTION('ref_axis',(-1.85863229568944E-16,1.,0.));
#4278=DIRECTION('center_axis',(-1.,-1.85863229568944E-16,0.));
#4279=DIRECTION('ref_axis',(-1.85863229568944E-16,1.,0.));
#4280=DIRECTION('center_axis',(-1.,-1.85863229568944E-16,0.));
#4281=DIRECTION('ref_axis',(-1.85863229568944E-16,1.,0.));
#4282=DIRECTION('center_axis',(-1.,-1.85863229568944E-16,0.));
#4283=DIRECTION('ref_axis',(-1.85863229568944E-16,1.,5.20417042793042E-15));
#4284=DIRECTION('center_axis',(-1.,-1.85863229568944E-16,0.));
#4285=DIRECTION('ref_axis',(-1.85863229568944E-16,1.,0.));
#4286=DIRECTION('center_axis',(-1.,-1.85863229568944E-16,-5.47382212626882E-48));
#4287=DIRECTION('ref_axis',(1.85863229568944E-16,-1.,1.01738225847426E-63));
#4288=DIRECTION('center_axis',(-1.,-1.85863229568944E-16,-5.47382212626882E-48));
#4289=DIRECTION('ref_axis',(1.85863229568944E-16,-1.,1.01738225847426E-63));
#4290=DIRECTION('center_axis',(-1.,-1.85863229568944E-16,-5.47382212626882E-48));
#4291=DIRECTION('ref_axis',(1.85863229568944E-16,-1.,1.01738225847426E-63));
#4292=DIRECTION('center_axis',(-1.,-1.85863229568944E-16,-5.47382212626882E-48));
#4293=DIRECTION('ref_axis',(1.85863229568944E-16,-1.,1.01738225847426E-63));
#4294=DIRECTION('center_axis',(-1.,-1.85863229568944E-16,-5.47382212626882E-48));
#4295=DIRECTION('ref_axis',(1.85863229568944E-16,-1.,1.01738225847426E-63));
#4296=DIRECTION('center_axis',(-1.,-1.85863229568944E-16,-5.47382212626882E-48));
#4297=DIRECTION('ref_axis',(1.85863229568944E-16,-1.,1.01738225847426E-63));
#4298=DIRECTION('center_axis',(-1.,-1.85863229568944E-16,-5.47382212626882E-48));
#4299=DIRECTION('ref_axis',(1.85863229568944E-16,-1.,1.01738225847426E-63));
#4300=DIRECTION('center_axis',(-1.,-1.85863229568944E-16,-5.47382212626882E-48));
#4301=DIRECTION('ref_axis',(1.85863229568944E-16,-1.,1.01738225847426E-63));
#4302=DIRECTION('axis',(0.,0.,1.));
#4303=DIRECTION('refdir',(1.,0.,0.));
#4304=DIRECTION('center_axis',(-1.,0.,0.));
#4305=DIRECTION('ref_axis',(0.,0.,1.));
#4306=DIRECTION('center_axis',(-1.,0.,0.));
#4307=DIRECTION('ref_axis',(0.,0.,1.));
#4308=DIRECTION('',(1.,0.,0.));
#4309=DIRECTION('center_axis',(-1.,0.,0.));
#4310=DIRECTION('ref_axis',(0.,0.,1.));
#4311=DIRECTION('center_axis',(-1.,0.,0.));
#4312=DIRECTION('ref_axis',(0.,0.,1.));
#4313=DIRECTION('center_axis',(-1.,0.,0.));
#4314=DIRECTION('ref_axis',(0.,0.,1.));
#4315=DIRECTION('',(-1.,0.,0.));
#4316=DIRECTION('center_axis',(-1.,0.,0.));
#4317=DIRECTION('ref_axis',(0.,0.,1.));
#4318=DIRECTION('center_axis',(1.,0.,0.));
#4319=DIRECTION('ref_axis',(0.,0.,-1.));
#4320=DIRECTION('center_axis',(-1.,0.,0.));
#4321=DIRECTION('ref_axis',(0.,0.,1.));
#4322=DIRECTION('axis',(0.,0.,1.));
#4323=DIRECTION('refdir',(1.,0.,0.));
#4324=DIRECTION('center_axis',(0.,0.,1.));
#4325=DIRECTION('ref_axis',(1.,0.,0.));
#4326=DIRECTION('center_axis',(0.,0.,-1.));
#4327=DIRECTION('ref_axis',(1.,0.,0.));
#4328=DIRECTION('',(0.,0.,1.));
#4329=DIRECTION('center_axis',(0.,0.,1.));
#4330=DIRECTION('ref_axis',(1.,0.,0.));
#4331=DIRECTION('center_axis',(1.,1.33440267382831E-16,0.));
#4332=DIRECTION('ref_axis',(-1.33440267382831E-16,1.,0.));
#4333=DIRECTION('',(1.33440267382831E-16,-1.,0.));
#4334=DIRECTION('',(0.,0.,1.));
#4335=DIRECTION('',(1.33440267382831E-16,-1.,0.));
#4336=DIRECTION('',(0.,0.,1.));
#4337=DIRECTION('center_axis',(0.,1.,0.));
#4338=DIRECTION('ref_axis',(0.,0.,1.));
#4339=DIRECTION('',(1.,0.,0.));
#4340=DIRECTION('',(0.,0.,1.));
#4341=DIRECTION('',(1.,0.,0.));
#4342=DIRECTION('',(0.,0.,1.));
#4343=DIRECTION('center_axis',(-1.,0.,0.));
#4344=DIRECTION('ref_axis',(0.,0.,1.));
#4345=DIRECTION('',(0.,1.,0.));
#4346=DIRECTION('',(0.,0.,1.));
#4347=DIRECTION('',(0.,1.,0.));
#4348=DIRECTION('',(0.,0.,1.));
#4349=DIRECTION('center_axis',(0.,-1.,0.));
#4350=DIRECTION('ref_axis',(0.,0.,-1.));
#4351=DIRECTION('',(-1.,0.,0.));
#4352=DIRECTION('',(0.,0.,1.));
#4353=DIRECTION('',(-1.,0.,0.));
#4354=DIRECTION('',(0.,0.,1.));
#4355=DIRECTION('center_axis',(0.,0.,1.));
#4356=DIRECTION('ref_axis',(1.,0.,0.));
#4357=DIRECTION('',(2.32848788721719E-16,1.,0.));
#4358=DIRECTION('',(1.,0.,0.));
#4359=DIRECTION('',(-1.,0.,0.));
#4360=DIRECTION('',(-2.32848788721719E-16,1.,0.));
#4361=DIRECTION('',(0.,-1.,0.));
#4362=DIRECTION('',(-1.,0.,0.));
#4363=DIRECTION('',(1.,0.,0.));
#4364=DIRECTION('',(0.,-1.,0.));
#4365=DIRECTION('center_axis',(0.,0.,1.));
#4366=DIRECTION('ref_axis',(1.,0.,0.));
#4367=DIRECTION('',(-1.,0.,0.));
#4368=DIRECTION('',(-2.32848788721719E-16,-1.,0.));
#4369=DIRECTION('',(0.,1.,0.));
#4370=DIRECTION('',(-1.,0.,0.));
#4371=DIRECTION('',(1.,0.,0.));
#4372=DIRECTION('',(0.,1.,0.));
#4373=DIRECTION('',(2.32848788721719E-16,-1.,0.));
#4374=DIRECTION('',(1.,0.,0.));
#4375=DIRECTION('center_axis',(0.,-1.,0.));
#4376=DIRECTION('ref_axis',(0.,0.,-1.));
#4377=DIRECTION('',(0.,0.,1.));
#4378=DIRECTION('center_axis',(-1.,0.,0.));
#4379=DIRECTION('ref_axis',(0.,0.,1.));
#4380=DIRECTION('center_axis',(-1.,0.,0.));
#4381=DIRECTION('ref_axis',(0.,0.,1.));
#4382=DIRECTION('',(0.,0.,1.));
#4383=DIRECTION('center_axis',(0.,1.,0.));
#4384=DIRECTION('ref_axis',(0.,0.,1.));
#4385=DIRECTION('center_axis',(0.,1.,0.));
#4386=DIRECTION('ref_axis',(0.,0.,1.));
#4387=DIRECTION('',(0.,0.,1.));
#4388=DIRECTION('center_axis',(1.,2.32848788721719E-16,0.));
#4389=DIRECTION('ref_axis',(-2.32848788721719E-16,1.,0.));
#4390=DIRECTION('center_axis',(1.,-2.32848788721719E-16,0.));
#4391=DIRECTION('ref_axis',(2.32848788721719E-16,1.,0.));
#4392=DIRECTION('',(0.,0.,1.));
#4393=DIRECTION('center_axis',(0.,-1.,0.));
#4394=DIRECTION('ref_axis',(0.,0.,-1.));
#4395=DIRECTION('axis',(0.,0.,1.));
#4396=DIRECTION('refdir',(1.,0.,0.));
#4397=DIRECTION('',(0.404889385483999,-6.75715337925259E-5,0.914365671357186));
#4398=DIRECTION('',(-0.404889387332683,-2.14111170223934E-15,0.914365673035337));
#4399=DIRECTION('',(0.404889385483998,6.75715337926642E-5,-0.914365671357186));
#4400=DIRECTION('',(-0.404889387332682,4.97544927214364E-16,-0.914365673035337));
#4401=DIRECTION('center_axis',(-1.,-1.83084271870903E-16,0.));
#4402=DIRECTION('ref_axis',(1.83084271870903E-16,-1.,0.));
#4403=DIRECTION('center_axis',(1.,0.,0.));
#4404=DIRECTION('ref_axis',(0.,0.,-1.));
#4405=DIRECTION('',(-1.,-1.83084271870903E-16,0.));
#4406=DIRECTION('center_axis',(-1.,-1.83084271870903E-16,0.));
#4407=DIRECTION('ref_axis',(1.83084271870903E-16,-1.,0.));
#4408=DIRECTION('',(1.,1.83084271870903E-16,0.));
#4409=DIRECTION('center_axis',(1.,0.,0.));
#4410=DIRECTION('ref_axis',(0.,0.,-1.));
#4411=DIRECTION('',(1.,1.83084271870903E-16,0.));
#4412=DIRECTION('center_axis',(1.,-4.57710679677258E-17,0.));
#4413=DIRECTION('ref_axis',(4.57710679677258E-17,1.,0.));
#4414=DIRECTION('center_axis',(1.,0.,0.));
#4415=DIRECTION('ref_axis',(0.,0.,-1.));
#4416=DIRECTION('',(-1.,-1.83084271870903E-16,0.));
#4417=DIRECTION('center_axis',(-1.,-1.83084271870903E-16,0.));
#4418=DIRECTION('ref_axis',(1.83084271870903E-16,-1.,0.));
#4419=DIRECTION('',(1.,1.83084271870903E-16,0.));
#4420=DIRECTION('center_axis',(0.,0.,1.));
#4421=DIRECTION('ref_axis',(1.,0.,0.));
#4422=DIRECTION('',(0.,0.,1.));
#4423=DIRECTION('center_axis',(0.,0.,-1.));
#4424=DIRECTION('ref_axis',(-1.,0.,0.));
#4425=DIRECTION('center_axis',(0.,0.,1.));
#4426=DIRECTION('ref_axis',(1.,0.,0.));
#4427=DIRECTION('center_axis',(1.42580011724121E-15,0.,1.));
#4428=DIRECTION('ref_axis',(1.,0.,-1.42580011724121E-15));
#4429=DIRECTION('',(0.,0.,1.));
#4430=DIRECTION('center_axis',(1.,-4.57710679677258E-17,0.));
#4431=DIRECTION('ref_axis',(4.57710679677258E-17,1.,0.));
#4432=DIRECTION('center_axis',(1.,-4.57710679677258E-17,0.));
#4433=DIRECTION('ref_axis',(4.57710679677258E-17,1.,0.));
#4434=DIRECTION('',(-1.,4.57710679677258E-17,0.));
#4435=DIRECTION('center_axis',(1.,-4.57710679677258E-17,0.));
#4436=DIRECTION('ref_axis',(4.57710679677258E-17,1.,0.));
#4437=DIRECTION('center_axis',(-1.,-1.83084271870902E-16,0.));
#4438=DIRECTION('ref_axis',(1.83084271870902E-16,-1.,0.));
#4439=DIRECTION('center_axis',(-1.,-1.83084271870902E-16,0.));
#4440=DIRECTION('ref_axis',(1.83084271870902E-16,-1.,0.));
#4441=DIRECTION('',(0.707106781186537,-0.707106781186558,8.65956056235506E-17));
#4442=DIRECTION('center_axis',(1.,1.83084271870903E-16,0.));
#4443=DIRECTION('ref_axis',(1.83084271870903E-16,-1.,0.));
#4444=DIRECTION('center_axis',(-1.,-1.83084271870903E-16,0.));
#4445=DIRECTION('ref_axis',(1.83084271870903E-16,-1.,0.));
#4446=DIRECTION('center_axis',(-1.,-1.83084271870903E-16,0.));
#4447=DIRECTION('ref_axis',(1.83084271870903E-16,-1.,0.));
#4448=DIRECTION('',(1.,1.83084271870903E-16,0.));
#4449=DIRECTION('center_axis',(-1.,-1.83084271870903E-16,0.));
#4450=DIRECTION('ref_axis',(1.83084271870903E-16,-1.,0.));
#4451=DIRECTION('center_axis',(-1.,-1.83084271870903E-16,0.));
#4452=DIRECTION('ref_axis',(1.83084271870903E-16,-1.,0.));
#4453=DIRECTION('',(1.,1.83084271870903E-16,0.));
#4454=DIRECTION('center_axis',(-1.,-1.83084271870903E-16,0.));
#4455=DIRECTION('ref_axis',(1.83084271870903E-16,-1.,0.));
#4456=DIRECTION('center_axis',(-1.,-1.83084271870903E-16,0.));
#4457=DIRECTION('ref_axis',(1.83084271870903E-16,-1.,0.));
#4458=DIRECTION('center_axis',(-1.,-1.83084271870903E-16,0.));
#4459=DIRECTION('ref_axis',(1.83084271870903E-16,-1.,0.));
#4460=DIRECTION('',(0.99522852511998,-0.0975714240313706,1.19490532128267E-17));
#4461=DIRECTION('center_axis',(-1.,-1.83084271870903E-16,0.));
#4462=DIRECTION('ref_axis',(1.83084271870903E-16,-1.,0.));
#4463=DIRECTION('center_axis',(-1.,-1.83084271870903E-16,0.));
#4464=DIRECTION('ref_axis',(1.83084271870903E-16,-1.,0.));
#4465=DIRECTION('center_axis',(1.,-4.57710679677258E-17,0.));
#4466=DIRECTION('ref_axis',(4.57710679677258E-17,1.,0.));
#4467=DIRECTION('',(1.,1.83084271870903E-16,0.));
#4468=DIRECTION('center_axis',(-1.,-1.83084271870903E-16,0.));
#4469=DIRECTION('ref_axis',(1.83084271870903E-16,-1.,0.));
#4470=DIRECTION('center_axis',(-1.,-1.83084271870903E-16,0.));
#4471=DIRECTION('ref_axis',(1.83084271870903E-16,-1.,0.));
#4472=DIRECTION('center_axis',(-1.,-1.83084271870903E-16,0.));
#4473=DIRECTION('ref_axis',(1.83084271870903E-16,-1.,0.));
#4474=DIRECTION('center_axis',(-1.,-1.83084271870903E-16,0.));
#4475=DIRECTION('ref_axis',(1.83084271870903E-16,-1.,0.));
#4476=DIRECTION('center_axis',(-1.,-1.83084271870903E-16,0.));
#4477=DIRECTION('ref_axis',(1.83084271870903E-16,-1.,0.));
#4478=DIRECTION('center_axis',(1.,-4.57710679677258E-17,0.));
#4479=DIRECTION('ref_axis',(4.57710679677258E-17,1.,0.));
#4480=DIRECTION('center_axis',(-1.,4.57710679677258E-17,0.));
#4481=DIRECTION('ref_axis',(-4.57710679677258E-17,-1.,0.));
#4482=DIRECTION('center_axis',(1.,1.83084271870903E-16,0.));
#4483=DIRECTION('ref_axis',(-1.83084271870903E-16,1.,0.));
#4484=DIRECTION('',(0.,1.,0.));
#4485=DIRECTION('center_axis',(1.42580011724121E-15,0.,1.));
#4486=DIRECTION('ref_axis',(1.,0.,-1.42580011724121E-15));
#4487=DIRECTION('',(0.,1.,0.));
#4488=DIRECTION('center_axis',(1.,0.,0.));
#4489=DIRECTION('ref_axis',(0.,0.,-1.));
#4490=DIRECTION('',(0.,1.,0.));
#4491=DIRECTION('center_axis',(0.,0.,-1.));
#4492=DIRECTION('ref_axis',(-1.,0.,0.));
#4493=DIRECTION('',(0.,1.,0.));
#4494=DIRECTION('center_axis',(1.,1.83084271870903E-16,0.));
#4495=DIRECTION('ref_axis',(-1.83084271870903E-16,1.,0.));
#4496=DIRECTION('axis',(0.,0.,1.));
#4497=DIRECTION('refdir',(1.,0.,0.));
#4498=DIRECTION('center_axis',(0.,0.,1.));
#4499=DIRECTION('ref_axis',(1.,0.,0.));
#4500=DIRECTION('center_axis',(0.,0.,-1.));
#4501=DIRECTION('ref_axis',(1.,0.,0.));
#4502=DIRECTION('',(0.,0.,-1.));
#4503=DIRECTION('center_axis',(0.,0.,1.));
#4504=DIRECTION('ref_axis',(1.,0.,0.));
#4505=DIRECTION('',(0.,0.,1.));
#4506=DIRECTION('center_axis',(0.,0.,1.));
#4507=DIRECTION('ref_axis',(1.,0.,0.));
#4508=DIRECTION('center_axis',(0.,0.,-1.));
#4509=DIRECTION('ref_axis',(1.,-1.78574475468201E-15,0.));
#4510=DIRECTION('',(0.,0.,1.));
#4511=DIRECTION('center_axis',(0.,0.,1.));
#4512=DIRECTION('ref_axis',(-1.,0.,0.));
#4513=DIRECTION('',(0.,0.,1.));
#4514=DIRECTION('center_axis',(0.,0.,-1.));
#4515=DIRECTION('ref_axis',(-5.0532154980743E-16,1.,0.));
#4516=DIRECTION('center_axis',(0.,0.,1.));
#4517=DIRECTION('ref_axis',(1.,0.,0.));
#4518=DIRECTION('',(0.,0.,-1.));
#4519=DIRECTION('center_axis',(0.,0.,1.));
#4520=DIRECTION('ref_axis',(1.,0.,0.));
#4521=DIRECTION('center_axis',(0.,0.,1.));
#4522=DIRECTION('ref_axis',(1.,0.,0.));
#4523=DIRECTION('center_axis',(0.,0.,-1.));
#4524=DIRECTION('ref_axis',(1.,0.,0.));
#4525=DIRECTION('center_axis',(0.,0.,1.));
#4526=DIRECTION('ref_axis',(1.,0.,0.));
#4527=DIRECTION('center_axis',(0.,0.,-1.));
#4528=DIRECTION('ref_axis',(-1.,0.,0.));
#4529=DIRECTION('center_axis',(0.,0.,1.));
#4530=DIRECTION('ref_axis',(1.,0.,0.));
#4531=DIRECTION('center_axis',(0.,0.,-1.));
#4532=DIRECTION('ref_axis',(1.,0.,0.));
#4533=DIRECTION('center_axis',(0.,0.,1.));
#4534=DIRECTION('ref_axis',(1.,0.,0.));
#4535=DIRECTION('center_axis',(0.,0.,-1.));
#4536=DIRECTION('ref_axis',(1.,0.,0.));
#4537=DIRECTION('center_axis',(0.,0.,1.));
#4538=DIRECTION('ref_axis',(1.,0.,0.));
#4539=DIRECTION('center_axis',(0.,0.,1.));
#4540=DIRECTION('ref_axis',(1.,0.,0.));
#4541=DIRECTION('center_axis',(0.,0.,-1.));
#4542=DIRECTION('ref_axis',(1.,1.78574475468201E-15,0.));
#4543=DIRECTION('center_axis',(0.,0.,1.));
#4544=DIRECTION('ref_axis',(1.,0.,0.));
#4545=DIRECTION('center_axis',(0.,0.,1.));
#4546=DIRECTION('ref_axis',(-0.791487217192215,0.61118572056399,0.));
#4547=DIRECTION('',(0.,0.,1.));
#4548=DIRECTION('',(0.,0.,1.));
#4549=DIRECTION('center_axis',(0.,0.,1.));
#4550=DIRECTION('ref_axis',(1.,0.,0.));
#4551=DIRECTION('center_axis',(0.,0.,1.));
#4552=DIRECTION('ref_axis',(1.,0.,0.));
#4553=DIRECTION('',(0.,0.,1.));
#4554=DIRECTION('center_axis',(0.,0.,1.));
#4555=DIRECTION('ref_axis',(1.,0.,0.));
#4556=DIRECTION('center_axis',(0.,0.,1.));
#4557=DIRECTION('ref_axis',(-0.504127969118338,-0.863628965906436,0.));
#4558=DIRECTION('axis',(0.,0.,1.));
#4559=DIRECTION('refdir',(1.,0.,0.));
#4560=DIRECTION('center_axis',(0.,-1.,0.));
#4561=DIRECTION('ref_axis',(0.,0.,-1.));
#4562=DIRECTION('center_axis',(0.,-1.,0.));
#4563=DIRECTION('ref_axis',(0.,0.,1.));
#4564=DIRECTION('',(-8.65956056235497E-17,-0.707106781186544,0.707106781186551));
#4565=DIRECTION('center_axis',(0.,1.,0.));
#4566=DIRECTION('ref_axis',(0.,0.,1.));
#4567=DIRECTION('center_axis',(0.,-1.,0.));
#4568=DIRECTION('ref_axis',(0.,0.,-1.));
#4569=DIRECTION('center_axis',(0.,-1.,0.));
#4570=DIRECTION('ref_axis',(0.,0.,-1.));
#4571=DIRECTION('',(0.,-1.,0.));
#4572=DIRECTION('center_axis',(0.,1.,0.));
#4573=DIRECTION('ref_axis',(0.,0.,1.));
#4574=DIRECTION('center_axis',(0.,-1.,0.));
#4575=DIRECTION('ref_axis',(0.,0.,1.));
#4576=DIRECTION('center_axis',(-0.948250947674427,-6.78917425016181E-14,
0.317521873631646));
#4577=DIRECTION('ref_axis',(-0.317521873631646,-4.81926486971319E-29,-0.948250947674427));
#4578=DIRECTION('center_axis',(0.,1.,0.));
#4579=DIRECTION('ref_axis',(0.,0.,1.));
#4580=DIRECTION('center_axis',(-0.94825094767444,0.,-0.317521873631608));
#4581=DIRECTION('ref_axis',(-0.317521873631608,0.,0.94825094767444));
#4582=DIRECTION('center_axis',(0.,-1.,0.));
#4583=DIRECTION('ref_axis',(0.,0.,-1.));
#4584=DIRECTION('center_axis',(8.67361737988396E-15,-1.,5.0077153291238E-15));
#4585=DIRECTION('ref_axis',(-1.,-8.673617379884E-15,-8.67361737988403E-15));
#4586=DIRECTION('',(0.,1.,0.));
#4587=DIRECTION('center_axis',(-3.25260651745648E-15,-1.,1.87789324842143E-15));
#4588=DIRECTION('ref_axis',(1.,-3.25260651745648E-15,-5.46506401086679E-44));
#4589=DIRECTION('',(0.,-1.,0.));
#4590=DIRECTION('center_axis',(0.,1.,0.));
#4591=DIRECTION('ref_axis',(0.,0.,1.));
#4592=DIRECTION('center_axis',(0.,-1.,0.));
#4593=DIRECTION('ref_axis',(0.,0.,-1.));
#4594=DIRECTION('center_axis',(-0.948250947674425,0.,0.317521873631651));
#4595=DIRECTION('ref_axis',(-0.317521873631651,4.33680868994201E-14,-0.948250947674425));
#4596=DIRECTION('center_axis',(0.,1.,0.));
#4597=DIRECTION('ref_axis',(0.,0.,1.));
#4598=DIRECTION('center_axis',(-0.948250947674424,-6.03274245433074E-14,
-0.317521873631656));
#4599=DIRECTION('ref_axis',(-0.317521873631656,1.27015359233011E-28,0.948250947674424));
#4600=DIRECTION('center_axis',(0.,1.,-6.12323399573676E-17));
#4601=DIRECTION('ref_axis',(0.,0.,-1.));
#4602=DIRECTION('center_axis',(0.,-1.,0.));
#4603=DIRECTION('ref_axis',(0.,0.,-1.));
#4604=DIRECTION('center_axis',(1.,0.,-1.22464679914735E-16));
#4605=DIRECTION('ref_axis',(1.22464679914735E-16,0.,1.));
#4606=DIRECTION('center_axis',(0.,-1.,0.));
#4607=DIRECTION('ref_axis',(0.,0.,-1.));
#4608=DIRECTION('center_axis',(0.,1.,0.));
#4609=DIRECTION('ref_axis',(0.,0.,1.));
#4610=DIRECTION('',(0.,1.,0.));
#4611=DIRECTION('center_axis',(-0.5,0.,-0.866025403784439));
#4612=DIRECTION('ref_axis',(0.866025403784439,0.,-0.5));
#4613=DIRECTION('center_axis',(0.,1.,0.));
#4614=DIRECTION('ref_axis',(0.,0.,1.));
#4615=DIRECTION('center_axis',(0.5,0.,-0.866025403784439));
#4616=DIRECTION('ref_axis',(-0.866025403784439,0.,-0.5));
#4617=DIRECTION('center_axis',(1.,0.,0.));
#4618=DIRECTION('ref_axis',(0.,0.,-1.));
#4619=DIRECTION('center_axis',(-0.5,0.,-0.866025403784439));
#4620=DIRECTION('ref_axis',(0.866025403784439,0.,-0.5));
#4621=DIRECTION('center_axis',(0.,1.,0.));
#4622=DIRECTION('ref_axis',(0.,0.,1.));
#4623=DIRECTION('center_axis',(-0.5,0.,0.866025403784439));
#4624=DIRECTION('ref_axis',(0.866025403784439,0.,0.5));
#4625=DIRECTION('center_axis',(-1.,0.,0.));
#4626=DIRECTION('ref_axis',(0.,0.,1.));
#4627=DIRECTION('center_axis',(0.5,0.,0.866025403784438));
#4628=DIRECTION('ref_axis',(0.866025403784439,0.,-0.5));
#4629=DIRECTION('center_axis',(0.,-1.,0.));
#4630=DIRECTION('ref_axis',(0.,0.,-1.));
#4631=DIRECTION('center_axis',(1.,0.,0.));
#4632=DIRECTION('ref_axis',(0.,0.,-1.));
#4633=DIRECTION('center_axis',(0.5,0.,-0.866025403784439));
#4634=DIRECTION('ref_axis',(-0.866025403784439,0.,-0.5));
#4635=DIRECTION('center_axis',(0.5,0.,0.866025403784438));
#4636=DIRECTION('ref_axis',(0.866025403784439,0.,-0.5));
#4637=DIRECTION('center_axis',(0.,-1.,0.));
#4638=DIRECTION('ref_axis',(0.,0.,-1.));
#4639=DIRECTION('center_axis',(-1.,0.,0.));
#4640=DIRECTION('ref_axis',(0.,0.,1.));
#4641=DIRECTION('center_axis',(-0.5,0.,0.866025403784439));
#4642=DIRECTION('ref_axis',(0.866025403784439,0.,0.5));
#4643=DIRECTION('center_axis',(-1.,0.,0.));
#4644=DIRECTION('ref_axis',(0.,0.,1.));
#4645=DIRECTION('',(0.,-1.,0.));
#4646=DIRECTION('center_axis',(-1.,0.,0.));
#4647=DIRECTION('ref_axis',(0.,0.,1.));
#4648=DIRECTION('',(0.,0.,1.));
#4649=DIRECTION('center_axis',(-1.,0.,0.));
#4650=DIRECTION('ref_axis',(0.,0.,1.));
#4651=DIRECTION('',(0.,1.,0.));
#4652=DIRECTION('center_axis',(-1.,0.,0.));
#4653=DIRECTION('ref_axis',(0.,0.,1.));
#4654=DIRECTION('',(0.,0.,-1.));
#4655=DIRECTION('center_axis',(-1.,0.,0.));
#4656=DIRECTION('ref_axis',(0.,0.,1.));
#4657=DIRECTION('center_axis',(-0.5,0.,0.866025403784439));
#4658=DIRECTION('ref_axis',(0.866025403784439,0.,0.5));
#4659=DIRECTION('center_axis',(-0.5,0.,0.866025403784439));
#4660=DIRECTION('ref_axis',(0.866025403784439,0.,0.5));
#4661=DIRECTION('',(0.866025403784439,0.,0.5));
#4662=DIRECTION('center_axis',(-0.5,0.,0.866025403784439));
#4663=DIRECTION('ref_axis',(0.866025403784439,0.,0.5));
#4664=DIRECTION('',(0.,1.,0.));
#4665=DIRECTION('center_axis',(-0.5,0.,0.866025403784439));
#4666=DIRECTION('ref_axis',(0.866025403784439,0.,0.5));
#4667=DIRECTION('',(-0.866025403784439,0.,-0.5));
#4668=DIRECTION('center_axis',(-0.5,0.,0.866025403784439));
#4669=DIRECTION('ref_axis',(0.866025403784439,0.,0.5));
#4670=DIRECTION('',(0.,-1.,0.));
#4671=DIRECTION('center_axis',(0.5,0.,0.866025403784439));
#4672=DIRECTION('ref_axis',(0.866025403784439,0.,-0.5));
#4673=DIRECTION('center_axis',(0.5,0.,0.866025403784439));
#4674=DIRECTION('ref_axis',(0.866025403784439,0.,-0.5));
#4675=DIRECTION('',(0.866025403784439,0.,-0.5));
#4676=DIRECTION('center_axis',(0.5,0.,0.866025403784439));
#4677=DIRECTION('ref_axis',(0.866025403784439,0.,-0.5));
#4678=DIRECTION('',(0.,1.,0.));
#4679=DIRECTION('center_axis',(0.5,0.,0.866025403784439));
#4680=DIRECTION('ref_axis',(0.866025403784439,0.,-0.5));
#4681=DIRECTION('',(-0.866025403784439,0.,0.5));
#4682=DIRECTION('center_axis',(0.5,0.,0.866025403784439));
#4683=DIRECTION('ref_axis',(0.866025403784439,0.,-0.5));
#4684=DIRECTION('',(0.,-1.,0.));
#4685=DIRECTION('center_axis',(1.,0.,0.));
#4686=DIRECTION('ref_axis',(0.,0.,-1.));
#4687=DIRECTION('center_axis',(1.,0.,0.));
#4688=DIRECTION('ref_axis',(0.,0.,-1.));
#4689=DIRECTION('',(0.,0.,1.));
#4690=DIRECTION('center_axis',(1.,0.,0.));
#4691=DIRECTION('ref_axis',(0.,0.,-1.));
#4692=DIRECTION('',(0.,-1.,0.));
#4693=DIRECTION('center_axis',(1.,0.,0.));
#4694=DIRECTION('ref_axis',(0.,0.,-1.));
#4695=DIRECTION('',(0.,0.,-1.));
#4696=DIRECTION('center_axis',(1.,0.,0.));
#4697=DIRECTION('ref_axis',(0.,0.,-1.));
#4698=DIRECTION('',(0.,1.,0.));
#4699=DIRECTION('center_axis',(0.5,0.,-0.866025403784439));
#4700=DIRECTION('ref_axis',(-0.866025403784439,0.,-0.5));
#4701=DIRECTION('center_axis',(0.5,0.,-0.866025403784439));
#4702=DIRECTION('ref_axis',(-0.866025403784439,0.,-0.5));
#4703=DIRECTION('',(0.866025403784439,0.,0.5));
#4704=DIRECTION('center_axis',(0.5,0.,-0.866025403784439));
#4705=DIRECTION('ref_axis',(-0.866025403784439,0.,-0.5));
#4706=DIRECTION('',(0.,-1.,0.));
#4707=DIRECTION('center_axis',(0.5,0.,-0.866025403784439));
#4708=DIRECTION('ref_axis',(-0.866025403784439,0.,-0.5));
#4709=DIRECTION('',(-0.866025403784439,0.,-0.5));
#4710=DIRECTION('center_axis',(0.5,0.,-0.866025403784439));
#4711=DIRECTION('ref_axis',(-0.866025403784439,0.,-0.5));
#4712=DIRECTION('center_axis',(-0.5,0.,-0.866025403784439));
#4713=DIRECTION('ref_axis',(-0.866025403784439,0.,0.5));
#4714=DIRECTION('center_axis',(-0.5,0.,-0.866025403784439));
#4715=DIRECTION('ref_axis',(-0.866025403784439,0.,0.5));
#4716=DIRECTION('',(0.866025403784439,0.,-0.5));
#4717=DIRECTION('center_axis',(-0.5,0.,-0.866025403784439));
#4718=DIRECTION('ref_axis',(-0.866025403784439,0.,0.5));
#4719=DIRECTION('center_axis',(-0.5,0.,-0.866025403784439));
#4720=DIRECTION('ref_axis',(-0.866025403784439,0.,0.5));
#4721=DIRECTION('',(-0.866025403784439,0.,0.5));
#4722=DIRECTION('center_axis',(-0.5,0.,-0.866025403784439));
#4723=DIRECTION('ref_axis',(-0.866025403784439,0.,0.5));
#4724=DIRECTION('',(0.,1.,0.));
#4725=DIRECTION('center_axis',(0.,1.,0.));
#4726=DIRECTION('ref_axis',(0.,0.,1.));
#4727=DIRECTION('center_axis',(0.,-1.,0.));
#4728=DIRECTION('ref_axis',(8.88178419700125E-16,0.,1.));
#4729=DIRECTION('',(0.,0.,1.));
#4730=DIRECTION('center_axis',(0.,1.,0.));
#4731=DIRECTION('ref_axis',(0.,0.,1.));
#4732=DIRECTION('',(0.866025403784439,0.,0.5));
#4733=DIRECTION('',(0.866025403784439,0.,-0.5));
#4734=DIRECTION('center_axis',(0.,1.,0.));
#4735=DIRECTION('ref_axis',(0.,0.,1.));
#4736=DIRECTION('',(0.,0.,-1.));
#4737=DIRECTION('center_axis',(0.,1.,0.));
#4738=DIRECTION('ref_axis',(0.,0.,1.));
#4739=DIRECTION('',(-0.866025403784439,0.,-0.5));
#4740=DIRECTION('center_axis',(0.,1.,0.));
#4741=DIRECTION('ref_axis',(0.,0.,1.));
#4742=DIRECTION('',(-0.866025403784439,0.,0.5));
#4743=DIRECTION('center_axis',(0.,1.,0.));
#4744=DIRECTION('ref_axis',(0.,0.,1.));
#4745=DIRECTION('',(0.,0.,1.));
#4746=DIRECTION('center_axis',(0.,-1.,0.));
#4747=DIRECTION('ref_axis',(-8.88178419700125E-16,0.,1.));
#4748=DIRECTION('',(-0.866025403784439,0.,0.5));
#4749=DIRECTION('',(-0.866025403784439,0.,-0.5));
#4750=DIRECTION('center_axis',(0.,-1.,0.));
#4751=DIRECTION('ref_axis',(0.,0.,1.));
#4752=DIRECTION('',(0.,0.,-1.));
#4753=DIRECTION('center_axis',(0.,-1.,0.));
#4754=DIRECTION('ref_axis',(0.,0.,1.));
#4755=DIRECTION('',(0.866025403784439,0.,-0.5));
#4756=DIRECTION('center_axis',(0.,-1.,0.));
#4757=DIRECTION('ref_axis',(1.77635683940025E-15,0.,1.));
#4758=DIRECTION('',(0.866025403784439,0.,0.5));
#4759=DIRECTION('center_axis',(0.,-1.,0.));
#4760=DIRECTION('ref_axis',(0.,0.,1.));
#4761=DIRECTION('center_axis',(0.5,0.,0.866025403784438));
#4762=DIRECTION('ref_axis',(0.866025403784439,0.,-0.5));
#4763=DIRECTION('center_axis',(0.5,0.,-0.866025403784439));
#4764=DIRECTION('ref_axis',(-0.866025403784439,0.,-0.5));
#4765=DIRECTION('center_axis',(-0.5,0.,-0.866025403784439));
#4766=DIRECTION('ref_axis',(-0.866025403784439,0.,0.5));
#4767=DIRECTION('center_axis',(0.5,0.,0.866025403784438));
#4768=DIRECTION('ref_axis',(0.866025403784439,0.,-0.5));
#4769=DIRECTION('center_axis',(-0.5,0.,-0.866025403784439));
#4770=DIRECTION('ref_axis',(-0.866025403784439,0.,0.5));
#4771=DIRECTION('center_axis',(-1.,0.,0.));
#4772=DIRECTION('ref_axis',(0.,0.,1.));
#4773=DIRECTION('center_axis',(0.,-1.,0.));
#4774=DIRECTION('ref_axis',(0.,0.,-1.));
#4775=DIRECTION('center_axis',(0.5,0.,0.866025403784438));
#4776=DIRECTION('ref_axis',(0.866025403784439,0.,-0.5));
#4777=DIRECTION('center_axis',(-0.5,0.,0.866025403784439));
#4778=DIRECTION('ref_axis',(0.866025403784439,0.,0.5));
#4779=DIRECTION('center_axis',(0.5,0.,0.866025403784439));
#4780=DIRECTION('ref_axis',(0.866025403784439,0.,-0.5));
#4781=DIRECTION('center_axis',(0.,-1.,0.));
#4782=DIRECTION('ref_axis',(0.,0.,-1.));
#4783=DIRECTION('center_axis',(0.5,0.,0.866025403784438));
#4784=DIRECTION('ref_axis',(0.866025403784439,0.,-0.5));
#4785=DIRECTION('center_axis',(1.,0.,0.));
#4786=DIRECTION('ref_axis',(0.,0.,-1.));
#4787=DIRECTION('center_axis',(0.5,0.,0.866025403784439));
#4788=DIRECTION('ref_axis',(0.866025403784439,0.,-0.5));
#4789=DIRECTION('center_axis',(-0.5,0.,-0.866025403784439));
#4790=DIRECTION('ref_axis',(0.866025403784439,0.,-0.5));
#4791=DIRECTION('center_axis',(-0.5,0.,-0.866025403784439));
#4792=DIRECTION('ref_axis',(-0.866025403784439,0.,0.5));
#4793=DIRECTION('center_axis',(0.5,0.,-0.866025403784439));
#4794=DIRECTION('ref_axis',(-0.866025403784439,0.,-0.5));
#4795=DIRECTION('center_axis',(-0.5,0.,-0.866025403784439));
#4796=DIRECTION('ref_axis',(0.866025403784439,0.,-0.5));
#4797=DIRECTION('center_axis',(0.,1.,0.));
#4798=DIRECTION('ref_axis',(0.,0.,1.));
#4799=DIRECTION('center_axis',(-1.,0.,0.));
#4800=DIRECTION('ref_axis',(0.,0.,1.));
#4801=DIRECTION('center_axis',(-0.5,0.,-0.866025403784439));
#4802=DIRECTION('ref_axis',(-0.866025403784439,0.,0.5));
#4803=DIRECTION('center_axis',(-0.5,0.,-0.866025403784439));
#4804=DIRECTION('ref_axis',(0.866025403784439,0.,-0.5));
#4805=DIRECTION('center_axis',(0.,1.,0.));
#4806=DIRECTION('ref_axis',(0.,0.,1.));
#4807=DIRECTION('center_axis',(0.5,0.,0.866025403784439));
#4808=DIRECTION('ref_axis',(0.866025403784439,0.,-0.5));
#4809=DIRECTION('center_axis',(-0.5,0.,0.866025403784439));
#4810=DIRECTION('ref_axis',(0.866025403784439,0.,0.5));
#4811=DIRECTION('center_axis',(-0.5,0.,-0.866025403784439));
#4812=DIRECTION('ref_axis',(0.866025403784439,0.,-0.5));
#4813=DIRECTION('center_axis',(0.,1.,0.));
#4814=DIRECTION('ref_axis',(0.,0.,1.));
#4815=DIRECTION('center_axis',(1.,0.,0.));
#4816=DIRECTION('ref_axis',(0.,0.,-1.));
#4817=DIRECTION('center_axis',(0.5,0.,0.866025403784439));
#4818=DIRECTION('ref_axis',(0.866025403784439,0.,-0.5));
#4819=DIRECTION('center_axis',(0.,1.,0.));
#4820=DIRECTION('ref_axis',(1.,0.,0.));
#4821=DIRECTION('center_axis',(-5.17751283984664E-14,-0.1010864170244,0.994877648906221));
#4822=DIRECTION('ref_axis',(-4.05998175189893E-29,0.994877648906221,0.1010864170244));
#4823=DIRECTION('center_axis',(0.,-7.15573433840431E-14,-1.));
#4824=DIRECTION('ref_axis',(0.,-1.,7.15573433840431E-14));
#4825=DIRECTION('center_axis',(-0.199143465014893,0.,0.979970346664562));
#4826=DIRECTION('ref_axis',(-0.979970346664562,-8.67361737988404E-15,-0.199143465014893));
#4827=DIRECTION('center_axis',(0.,0.,1.));
#4828=DIRECTION('ref_axis',(1.,0.,0.));
#4829=DIRECTION('center_axis',(-7.15573433840431E-14,0.,-1.));
#4830=DIRECTION('ref_axis',(-1.,0.,7.15573433840431E-14));
#4831=DIRECTION('center_axis',(0.,1.,0.));
#4832=DIRECTION('ref_axis',(0.,0.,1.));
#4833=DIRECTION('center_axis',(-0.749107482659445,-7.02110417793331E-14,
0.662448473032906));
#4834=DIRECTION('ref_axis',(0.662448473032906,2.48599189023735E-28,0.749107482659445));
#4835=DIRECTION('center_axis',(0.5,0.,0.866025403784439));
#4836=DIRECTION('ref_axis',(0.866025403784439,0.,-0.5));
#4837=DIRECTION('center_axis',(0.829541231031753,-0.287196439203378,-0.478935853040076));
#4838=DIRECTION('ref_axis',(-0.5,4.17395137324621E-16,-0.866025403784439));
#4839=DIRECTION('center_axis',(-0.861589317610118,0.101086417024454,0.497438824453107));
#4840=DIRECTION('ref_axis',(0.5,-2.3942973477981E-18,0.866025403784439));
#4841=DIRECTION('center_axis',(1.,0.,0.));
#4842=DIRECTION('ref_axis',(0.,0.,-1.));
#4843=DIRECTION('center_axis',(0.,-0.287196439203358,0.957871706080158));
#4844=DIRECTION('ref_axis',(0.,-0.957871706080157,-0.287196439203358));
#4845=DIRECTION('center_axis',(1.,0.,0.));
#4846=DIRECTION('ref_axis',(0.,0.,-1.));
#4847=DIRECTION('center_axis',(0.,0.101086417024377,0.994877648906223));
#4848=DIRECTION('ref_axis',(0.,-0.994877648906223,0.101086417024377));
#4849=DIRECTION('center_axis',(-1.41253933285967E-14,-0.287196439203367,
-0.957871706080155));
#4850=DIRECTION('ref_axis',(7.2563925722977E-30,0.957871706080155,-0.287196439203367));
#4851=DIRECTION('center_axis',(0.,1.,0.));
#4852=DIRECTION('ref_axis',(1.,0.,0.));
#4853=DIRECTION('center_axis',(-0.199143465014904,2.93519296686958E-14,
-0.97997034666456));
#4854=DIRECTION('ref_axis',(0.97997034666456,-1.27881005982267E-29,-0.199143465014904));
#4855=DIRECTION('center_axis',(0.,1.,0.));
#4856=DIRECTION('ref_axis',(1.,0.,0.));
#4857=DIRECTION('center_axis',(-0.866025403784418,0.,0.500000000000037));
#4858=DIRECTION('ref_axis',(-0.500000000000037,0.,-0.866025403784418));
#4859=DIRECTION('center_axis',(0.,1.,0.));
#4860=DIRECTION('ref_axis',(1.,0.,0.));
#4861=DIRECTION('center_axis',(0.,-1.,0.));
#4862=DIRECTION('ref_axis',(-8.67361737988405E-15,0.,1.));
#4863=DIRECTION('center_axis',(0.,1.,0.));
#4864=DIRECTION('ref_axis',(1.,0.,0.));
#4865=DIRECTION('center_axis',(0.,-1.,1.00154306582477E-14));
#4866=DIRECTION('ref_axis',(-8.67361737988405E-15,1.00154306582477E-14,
1.));
#4867=DIRECTION('center_axis',(-0.829541231031753,0.28719643920338,-0.478935853040074));
#4868=DIRECTION('ref_axis',(0.499999999999998,-5.90524342983604E-16,-0.866025403784439));
#4869=DIRECTION('center_axis',(0.5,0.,-0.866025403784439));
#4870=DIRECTION('ref_axis',(-0.866025403784439,0.,-0.5));
#4871=DIRECTION('center_axis',(-0.861589317610107,0.101086417024411,-0.497438824453135));
#4872=DIRECTION('ref_axis',(-0.500000000000025,-2.05653966383454E-16,0.866025403784424));
#4873=DIRECTION('center_axis',(0.,1.,0.));
#4874=DIRECTION('ref_axis',(0.,0.,1.));
#4875=DIRECTION('center_axis',(-0.749107482659488,0.,-0.662448473032858));
#4876=DIRECTION('ref_axis',(-0.662448473032858,0.,0.749107482659488));
#4877=DIRECTION('center_axis',(-0.866025403784439,0.,0.5));
#4878=DIRECTION('ref_axis',(0.5,0.,0.866025403784439));
#4879=DIRECTION('center_axis',(-0.86602540378444,3.49641228577842E-14,0.499999999999998));
#4880=DIRECTION('ref_axis',(0.499999999999998,-4.11195107519449E-31,0.86602540378444));
#4881=DIRECTION('center_axis',(0.,-1.,0.));
#4882=DIRECTION('ref_axis',(0.,0.,-1.));
#4883=DIRECTION('center_axis',(0.,-1.,1.75270036519335E-14));
#4884=DIRECTION('ref_axis',(0.,-1.75270036519335E-14,-1.));
#4885=DIRECTION('center_axis',(1.,0.,0.));
#4886=DIRECTION('ref_axis',(0.,0.,-1.));
#4887=DIRECTION('center_axis',(0.,-0.101086417024342,-0.994877648906227));
#4888=DIRECTION('ref_axis',(0.,0.994877648906226,-0.101086417024342));
#4889=DIRECTION('center_axis',(-1.47481513352255E-14,0.287196439203365,
0.957871706080155));
#4890=DIRECTION('ref_axis',(2.65299810676557E-29,-0.957871706080155,0.287196439203365));
#4891=DIRECTION('center_axis',(0.,0.,-1.));
#4892=DIRECTION('ref_axis',(-1.,0.,0.));
#4893=DIRECTION('center_axis',(0.,-1.14925430283463E-13,-1.));
#4894=DIRECTION('ref_axis',(0.,1.,-1.14925430283463E-13));
#4895=DIRECTION('center_axis',(-1.14925430283463E-13,0.,1.));
#4896=DIRECTION('ref_axis',(1.,0.,1.14925430283463E-13));
#4897=DIRECTION('center_axis',(1.,0.,0.));
#4898=DIRECTION('ref_axis',(0.,0.,-1.));
#4899=DIRECTION('center_axis',(0.,0.287196439203363,-0.957871706080156));
#4900=DIRECTION('ref_axis',(0.,0.957871706080156,0.287196439203362));
#4901=DIRECTION('center_axis',(5.33981346144544E-14,-0.101086417024396,
0.994877648906221));
#4902=DIRECTION('ref_axis',(1.43307595785059E-29,-0.994877648906221,-0.101086417024396));
#4903=DIRECTION('center_axis',(0.,-1.,0.));
#4904=DIRECTION('ref_axis',(0.,0.,-1.));
#4905=DIRECTION('center_axis',(-9.75781955236951E-15,-1.,-5.63367974526431E-15));
#4906=DIRECTION('ref_axis',(1.,-9.75781955236951E-15,1.12103877145985E-44));
#4907=DIRECTION('center_axis',(0.,1.,0.));
#4908=DIRECTION('ref_axis',(1.,0.,0.));
#4909=DIRECTION('center_axis',(-0.866025403784439,-6.18356505287836E-14,
-0.5));
#4910=DIRECTION('ref_axis',(0.5,1.71607915375628E-30,-0.866025403784439));
#4911=DIRECTION('center_axis',(0.,1.,0.));
#4912=DIRECTION('ref_axis',(1.,0.,0.));
#4913=DIRECTION('center_axis',(-0.86158931761011,-0.101086417024435,0.497438824453126));
#4914=DIRECTION('ref_axis',(-0.500000000000016,-8.82954564193182E-15,-0.866025403784429));
#4915=DIRECTION('center_axis',(0.,1.,0.));
#4916=DIRECTION('ref_axis',(1.,0.,0.));
#4917=DIRECTION('center_axis',(-0.829541231031755,-0.287196439203371,0.478935853040076));
#4918=DIRECTION('ref_axis',(-0.499999999999996,-9.54243899220994E-15,-0.866025403784441));
#4919=DIRECTION('center_axis',(0.,1.,0.));
#4920=DIRECTION('ref_axis',(1.,0.,0.));
#4921=DIRECTION('center_axis',(-0.199143465014924,-4.21017614145968E-14,
0.979970346664556));
#4922=DIRECTION('ref_axis',(-0.979970346664556,-2.71050543121381E-15,-0.199143465014924));
#4923=DIRECTION('center_axis',(0.,1.,0.));
#4924=DIRECTION('ref_axis',(1.,0.,0.));
#4925=DIRECTION('center_axis',(-0.199143465014975,0.,-0.979970346664546));
#4926=DIRECTION('ref_axis',(0.979970346664546,3.52365706057789E-15,-0.199143465014975));
#4927=DIRECTION('center_axis',(0.,1.,0.));
#4928=DIRECTION('ref_axis',(1.,0.,0.));
#4929=DIRECTION('center_axis',(-0.829541231031756,-0.28719643920338,-0.478935853040069));
#4930=DIRECTION('ref_axis',(0.499999999999997,-1.39967667904725E-14,-0.86602540378444));
#4931=DIRECTION('center_axis',(0.866025403784439,0.,0.5));
#4932=DIRECTION('ref_axis',(0.5,0.,-0.866025403784439));
#4933=DIRECTION('center_axis',(-0.866025403784458,0.,-0.499999999999966));
#4934=DIRECTION('ref_axis',(-0.499999999999966,0.,0.866025403784458));
#4935=DIRECTION('center_axis',(-0.5,0.,0.866025403784439));
#4936=DIRECTION('ref_axis',(0.866025403784439,0.,0.5));
#4937=DIRECTION('center_axis',(0.829541231031765,-0.287196439203365,0.478935853040062));
#4938=DIRECTION('ref_axis',(0.499999999999983,-1.74562014011744E-16,-0.866025403784448));
#4939=DIRECTION('center_axis',(-0.861589317610119,0.101086417024448,-0.497438824453106));
#4940=DIRECTION('ref_axis',(-0.499999999999998,7.745902403892E-18,0.86602540378444));
#4941=DIRECTION('center_axis',(0.5,0.,0.866025403784439));
#4942=DIRECTION('ref_axis',(0.866025403784439,0.,-0.5));
#4943=DIRECTION('center_axis',(-0.829541231031758,-0.287196439203359,0.478935853040078));
#4944=DIRECTION('ref_axis',(0.499999999999999,2.51520075033803E-16,0.866025403784439));
#4945=DIRECTION('center_axis',(0.5,0.,0.866025403784439));
#4946=DIRECTION('ref_axis',(0.866025403784439,0.,-0.5));
#4947=DIRECTION('center_axis',(-0.861589317610127,-0.101086417024433,0.497438824453096));
#4948=DIRECTION('ref_axis',(0.499999999999987,8.21668458334066E-17,0.866025403784446));
#4949=DIRECTION('center_axis',(0.,1.,0.));
#4950=DIRECTION('ref_axis',(0.,0.,1.));
#4951=DIRECTION('center_axis',(-0.74910748265946,0.,0.662448473032889));
#4952=DIRECTION('ref_axis',(0.662448473032889,0.,0.74910748265946));
#4953=DIRECTION('center_axis',(0.,1.,0.));
#4954=DIRECTION('ref_axis',(0.,0.,1.));
#4955=DIRECTION('center_axis',(-0.749107482659464,5.54706567608847E-14,
-0.662448473032884));
#4956=DIRECTION('ref_axis',(-0.662448473032884,1.32414025723286E-28,0.749107482659464));
#4957=DIRECTION('center_axis',(0.5,0.,-0.866025403784439));
#4958=DIRECTION('ref_axis',(-0.866025403784439,0.,-0.5));
#4959=DIRECTION('center_axis',(-0.861589317610122,-0.101086417024408,-0.49743882445311));
#4960=DIRECTION('ref_axis',(-0.5,-7.15092813094045E-18,0.866025403784439));
#4961=DIRECTION('center_axis',(0.5,0.,-0.866025403784439));
#4962=DIRECTION('ref_axis',(-0.866025403784439,0.,-0.5));
#4963=DIRECTION('center_axis',(0.861589317610122,0.101086417024421,0.497438824453108));
#4964=DIRECTION('ref_axis',(0.499999999999998,7.16296697270556E-18,-0.86602540378444));
#4965=DIRECTION('center_axis',(-0.829541231031761,-0.287196439203368,-0.478935853040068));
#4966=DIRECTION('ref_axis',(-0.49999999999999,4.4460279883491E-16,0.866025403784444));
#4967=DIRECTION('center_axis',(0.,1.,0.));
#4968=DIRECTION('ref_axis',(1.,0.,0.));
#4969=DIRECTION('center_axis',(-0.948250947674409,3.63509986091514E-14,
-0.317521873631701));
#4970=DIRECTION('ref_axis',(0.317521873631701,-3.81262645548618E-29,-0.948250947674409));
#4971=DIRECTION('center_axis',(0.,1.,0.));
#4972=DIRECTION('ref_axis',(1.,0.,0.));
#4973=DIRECTION('center_axis',(-0.866025403784459,0.,-0.499999999999965));
#4974=DIRECTION('ref_axis',(0.499999999999965,0.,-0.866025403784459));
#4975=DIRECTION('center_axis',(6.1232339957368E-17,1.,0.));
#4976=DIRECTION('ref_axis',(1.,0.,0.));
#4977=DIRECTION('center_axis',(8.67361737988401E-15,-1.,5.00771532912383E-15));
#4978=DIRECTION('ref_axis',(-1.,-8.67361737988387E-15,2.60208521396521E-14));
#4979=DIRECTION('center_axis',(0.,1.,0.));
#4980=DIRECTION('ref_axis',(1.,0.,0.));
#4981=DIRECTION('center_axis',(-0.866025403784439,3.43831006646852E-14,
0.5));
#4982=DIRECTION('ref_axis',(-0.5,2.49525696807541E-30,-0.866025403784439));
#4983=DIRECTION('center_axis',(0.,1.,0.));
#4984=DIRECTION('ref_axis',(1.,0.,0.));
#4985=DIRECTION('center_axis',(-0.866025403784404,0.,-0.500000000000061));
#4986=DIRECTION('ref_axis',(0.500000000000061,0.,-0.866025403784404));
#4987=DIRECTION('center_axis',(6.1232339957368E-17,1.,0.));
#4988=DIRECTION('ref_axis',(1.,0.,0.));
#4989=DIRECTION('center_axis',(-0.829541231031754,0.287196439203375,0.478935853040075));
#4990=DIRECTION('ref_axis',(-0.499999999999992,2.58221544109979E-14,-0.866025403784443));
#4991=DIRECTION('center_axis',(-0.5,0.,-0.866025403784439));
#4992=DIRECTION('ref_axis',(-0.866025403784439,0.,0.5));
#4993=DIRECTION('center_axis',(-0.86158931761011,0.101086417024435,0.497438824453126));
#4994=DIRECTION('ref_axis',(0.500000000000017,-2.46607843488102E-16,0.866025403784429));
#4995=DIRECTION('center_axis',(0.,1.,0.));
#4996=DIRECTION('ref_axis',(1.22464679914735E-16,0.,-1.));
#4997=DIRECTION('center_axis',(-0.948250947674425,0.,0.317521873631651));
#4998=DIRECTION('ref_axis',(0.317521873631651,0.,0.948250947674425));
#4999=DIRECTION('center_axis',(0.,1.,0.));
#5000=DIRECTION('ref_axis',(0.,0.,1.));
#5001=DIRECTION('center_axis',(0.749107482659426,0.,0.662448473032928));
#5002=DIRECTION('ref_axis',(0.662448473032928,0.,-0.749107482659426));
#5003=DIRECTION('center_axis',(-0.199143465014904,-2.93519296686958E-14,
-0.97997034666456));
#5004=DIRECTION('ref_axis',(-0.97997034666456,-1.27881005982267E-29,0.199143465014904));
#5005=DIRECTION('center_axis',(-0.866025403784439,0.,-0.5));
#5006=DIRECTION('ref_axis',(-0.5,0.,0.866025403784439));
#5007=DIRECTION('center_axis',(-0.866025403784439,4.6812504541412E-14,-0.5));
#5008=DIRECTION('ref_axis',(-0.5,5.19337291326334E-30,0.866025403784439));
#5009=DIRECTION('center_axis',(0.,-1.,0.));
#5010=DIRECTION('ref_axis',(-1.65389215948552E-15,0.,1.));
#5011=DIRECTION('center_axis',(-9.75781955236951E-15,-1.,5.63367974526431E-15));
#5012=DIRECTION('ref_axis',(1.,-9.75781955236951E-15,-1.68155815718978E-43));
#5013=DIRECTION('center_axis',(0.5,0.,0.866025403784439));
#5014=DIRECTION('ref_axis',(0.866025403784439,0.,-0.5));
#5015=DIRECTION('center_axis',(0.861589317610114,-0.101086417024512,-0.497438824453103));
#5016=DIRECTION('ref_axis',(-0.499999999999998,6.37095659320221E-18,-0.86602540378444));
#5017=DIRECTION('center_axis',(-0.829541231031761,0.287196439203367,0.478935853040068));
#5018=DIRECTION('ref_axis',(0.49999999999999,4.16045429843481E-16,0.866025403784444));
#5019=DIRECTION('center_axis',(0.866025403784439,0.,-0.5));
#5020=DIRECTION('ref_axis',(-0.5,0.,-0.866025403784439));
#5021=DIRECTION('center_axis',(-0.866025403784432,0.,0.500000000000011));
#5022=DIRECTION('ref_axis',(0.500000000000011,0.,0.866025403784432));
#5023=DIRECTION('center_axis',(-0.866025403784439,0.,-0.5));
#5024=DIRECTION('ref_axis',(-0.5,0.,0.866025403784439));
#5025=DIRECTION('center_axis',(-0.86602540378444,-7.18061389639901E-14,
-0.499999999999998));
#5026=DIRECTION('ref_axis',(-0.499999999999998,-1.36530950454694E-29,0.86602540378444));
#5027=DIRECTION('center_axis',(0.5,0.,-0.866025403784439));
#5028=DIRECTION('ref_axis',(-0.866025403784439,0.,-0.5));
#5029=DIRECTION('center_axis',(-0.829541231031757,0.287196439203362,-0.478935853040077));
#5030=DIRECTION('ref_axis',(-0.499999999999999,2.55714797234654E-16,0.866025403784439));
#5031=DIRECTION('center_axis',(0.861589317610141,-0.101086417024404,0.497438824453078));
#5032=DIRECTION('ref_axis',(0.499999999999968,3.57293483672415E-18,-0.866025403784457));
#5033=DIRECTION('center_axis',(0.,1.,0.));
#5034=DIRECTION('ref_axis',(1.,0.,0.));
#5035=DIRECTION('center_axis',(-0.86602540378444,-3.49641228577842E-14,
0.499999999999998));
#5036=DIRECTION('ref_axis',(-0.499999999999998,-4.11195107519449E-31,-0.86602540378444));
#5037=DIRECTION('center_axis',(0.,1.,0.));
#5038=DIRECTION('ref_axis',(-0.994979986397824,0.,-0.100074105880518));
#5039=DIRECTION('center_axis',(0.,-0.101086417024377,0.994877648906223));
#5040=DIRECTION('ref_axis',(-8.673617379884E-15,0.994877648906223,0.101086417024377));
#5041=DIRECTION('center_axis',(-7.15573433840431E-14,0.,-1.));
#5042=DIRECTION('ref_axis',(1.,0.,-7.15573433840431E-14));
#5043=DIRECTION('center_axis',(0.,1.,0.));
#5044=DIRECTION('ref_axis',(1.,0.,0.));
#5045=DIRECTION('center_axis',(-0.861589317610132,-0.101086417024438,-0.497438824453087));
#5046=DIRECTION('ref_axis',(0.499999999999978,-2.08058901956142E-16,-0.866025403784451));
#5047=DIRECTION('center_axis',(6.12323399573678E-17,1.,0.));
#5048=DIRECTION('ref_axis',(1.,0.,0.));
#5049=DIRECTION('center_axis',(-0.82954123103176,-0.287196439203352,-0.478935853040079));
#5050=DIRECTION('ref_axis',(0.499999999999995,1.40437046887256E-14,-0.866025403784441));
#5051=DIRECTION('center_axis',(0.,1.,0.));
#5052=DIRECTION('ref_axis',(1.,0.,0.));
#5053=DIRECTION('center_axis',(0.,1.,0.));
#5054=DIRECTION('ref_axis',(1.,0.,0.));
#5055=DIRECTION('center_axis',(-0.948250947674411,0.,-0.317521873631694));
#5056=DIRECTION('ref_axis',(0.317521873631694,1.24683249835833E-14,-0.948250947674411));
#5057=DIRECTION('center_axis',(6.12323399573678E-17,1.,0.));
#5058=DIRECTION('ref_axis',(1.,0.,0.));
#5059=DIRECTION('center_axis',(-0.829541231031755,-0.287196439203371,0.478935853040075));
#5060=DIRECTION('ref_axis',(-0.499999999999998,-1.76231351345845E-16,-0.86602540378444));
#5061=DIRECTION('center_axis',(0.866025403784439,0.,-0.5));
#5062=DIRECTION('ref_axis',(-0.5,0.,-0.866025403784439));
#5063=DIRECTION('center_axis',(-0.864858564672233,-0.0505745605773519,0.499461587046984));
#5064=DIRECTION('ref_axis',(-0.500089321311808,-0.000278942162528612,-0.865973783033392));
#5065=DIRECTION('center_axis',(0.,0.,-1.));
#5066=DIRECTION('ref_axis',(-1.,0.,0.));
#5067=DIRECTION('center_axis',(0.000117146476148524,-0.0505745644176246,
-0.998720281014995));
#5068=DIRECTION('ref_axis',(-0.446156523227928,0.893807017247891,-0.0453141556204722));
#5069=DIRECTION('center_axis',(-1.,0.,0.));
#5070=DIRECTION('ref_axis',(0.,0.,1.));
#5071=DIRECTION('center_axis',(1.99425739796376E-14,-0.287196439203364,
0.957871706080156));
#5072=DIRECTION('ref_axis',(-1.63640921780907E-29,-0.957871706080156,-0.287196439203364));
#5073=DIRECTION('center_axis',(-0.5,0.,0.866025403784439));
#5074=DIRECTION('ref_axis',(0.866025403784439,0.,0.5));
#5075=DIRECTION('center_axis',(-0.829541231031752,-0.287196439203385,-0.478935853040072));
#5076=DIRECTION('ref_axis',(-0.499999999999997,1.26305293957536E-17,0.866025403784441));
#5077=DIRECTION('center_axis',(-0.5,0.,0.866025403784439));
#5078=DIRECTION('ref_axis',(0.866025403784439,0.,0.5));
#5079=DIRECTION('center_axis',(-0.861589317610078,-0.101086417024462,-0.497438824453176));
#5080=DIRECTION('ref_axis',(-0.500000000000069,4.95586472996822E-17,0.866025403784399));
#5081=DIRECTION('center_axis',(0.,1.,0.));
#5082=DIRECTION('ref_axis',(1.01064309961486E-15,0.,-1.));
#5083=DIRECTION('center_axis',(-0.948250947674425,6.51376792599937E-14,
0.317521873631651));
#5084=DIRECTION('ref_axis',(0.317521873631651,-1.16313243025547E-28,0.948250947674425));
#5085=DIRECTION('center_axis',(-0.5,0.,-0.866025403784439));
#5086=DIRECTION('ref_axis',(-0.866025403784439,0.,0.5));
#5087=DIRECTION('center_axis',(-0.861589317610114,-0.101086417024508,0.497438824453103));
#5088=DIRECTION('ref_axis',(0.499999999999998,6.17150082144409E-18,0.86602540378444));
#5089=DIRECTION('center_axis',(-0.5,0.,-0.866025403784439));
#5090=DIRECTION('ref_axis',(-0.866025403784439,0.,0.5));
#5091=DIRECTION('center_axis',(-0.829541231031752,-0.287196439203378,0.478935853040076));
#5092=DIRECTION('ref_axis',(0.5,5.39313107558868E-16,0.866025403784438));
#5093=DIRECTION('center_axis',(-1.,0.,0.));
#5094=DIRECTION('ref_axis',(0.,0.,1.));
#5095=DIRECTION('center_axis',(0.,-0.287196439203354,-0.957871706080159));
#5096=DIRECTION('ref_axis',(0.,0.957871706080159,-0.287196439203354));
#5097=DIRECTION('center_axis',(0.,1.,0.));
#5098=DIRECTION('ref_axis',(1.,0.,0.));
#5099=DIRECTION('center_axis',(0.,-1.,-2.00308613164954E-14));
#5100=DIRECTION('ref_axis',(0.,-2.00308613164954E-14,1.));
#5101=DIRECTION('center_axis',(0.,1.,0.));
#5102=DIRECTION('ref_axis',(1.,0.,0.));
#5103=DIRECTION('center_axis',(-0.86602540378444,-3.1747643037438E-15,-0.499999999999998));
#5104=DIRECTION('ref_axis',(0.499999999999998,5.34273510922176E-31,-0.86602540378444));
#5105=DIRECTION('center_axis',(0.,1.,0.));
#5106=DIRECTION('ref_axis',(1.,0.,0.));
#5107=DIRECTION('center_axis',(-0.866025403784432,0.,0.500000000000011));
#5108=DIRECTION('ref_axis',(-0.500000000000011,0.,-0.866025403784432));
#5109=DIRECTION('center_axis',(0.,1.,0.));
#5110=DIRECTION('ref_axis',(-0.866025403784434,0.,-0.500000000000007));
#5111=DIRECTION('center_axis',(-8.67361737988407E-15,-1.,5.00771532912386E-15));
#5112=DIRECTION('ref_axis',(-1.,8.67361737988407E-15,-2.69049305150365E-43));
#5113=DIRECTION('center_axis',(0.,-1.,0.));
#5114=DIRECTION('ref_axis',(0.,0.,-1.));
#5115=DIRECTION('center_axis',(5.42101086242751E-15,-1.,3.12982208070238E-15));
#5116=DIRECTION('ref_axis',(1.,5.42101086242751E-15,0.));
#5117=DIRECTION('center_axis',(-0.5,0.,0.866025403784439));
#5118=DIRECTION('ref_axis',(0.866025403784439,0.,0.5));
#5119=DIRECTION('center_axis',(0.861589317610118,-0.101086417024453,0.497438824453107));
#5120=DIRECTION('ref_axis',(0.5,-7.47725293442112E-18,-0.866025403784439));
#5121=DIRECTION('center_axis',(-0.829541231031759,0.287196439203384,-0.478935853040061));
#5122=DIRECTION('ref_axis',(-0.499999999999986,-7.38722988415026E-16,0.866025403784447));
#5123=DIRECTION('center_axis',(0.866025403784439,0.,0.5));
#5124=DIRECTION('ref_axis',(0.5,0.,-0.866025403784439));
#5125=DIRECTION('center_axis',(-0.866025403784437,0.,-0.500000000000003));
#5126=DIRECTION('ref_axis',(-0.500000000000003,0.,0.866025403784437));
#5127=DIRECTION('center_axis',(-0.866025403784439,0.,0.5));
#5128=DIRECTION('ref_axis',(0.5,0.,0.866025403784439));
#5129=DIRECTION('center_axis',(-0.866025403784439,-3.43831006646852E-14,
0.5));
#5130=DIRECTION('ref_axis',(0.5,2.49525696807541E-30,0.866025403784439));
#5131=DIRECTION('center_axis',(-0.5,0.,-0.866025403784439));
#5132=DIRECTION('ref_axis',(-0.866025403784439,0.,0.5));
#5133=DIRECTION('center_axis',(-0.829541231031752,0.287196439203382,0.478935853040074));
#5134=DIRECTION('ref_axis',(0.499999999999998,-5.7450135142724E-16,0.866025403784439));
#5135=DIRECTION('center_axis',(0.861589317610127,-0.101086417024433,-0.497438824453096));
#5136=DIRECTION('ref_axis',(-0.499999999999987,8.21668458334066E-17,-0.866025403784446));
#5137=DIRECTION('center_axis',(0.,-1.,0.));
#5138=DIRECTION('ref_axis',(0.,0.,-1.));
#5139=DIRECTION('center_axis',(0.,-1.,-1.12673594905287E-14));
#5140=DIRECTION('ref_axis',(0.,1.12673594905287E-14,-1.));
#5141=DIRECTION('center_axis',(0.,1.,0.));
#5142=DIRECTION('ref_axis',(1.,0.,0.));
#5143=DIRECTION('center_axis',(0.,-0.287196439203347,-0.957871706080161));
#5144=DIRECTION('ref_axis',(-8.67361737988404E-15,-0.957871706080161,0.287196439203347));
#5145=DIRECTION('center_axis',(0.,1.,0.));
#5146=DIRECTION('ref_axis',(1.,0.,0.));
#5147=DIRECTION('center_axis',(-0.749107482659497,-3.02324171289191E-14,
-0.662448473032847));
#5148=DIRECTION('ref_axis',(0.662448473032847,1.76182853028899E-15,-0.749107482659497));
#5149=DIRECTION('center_axis',(0.,1.,0.));
#5150=DIRECTION('ref_axis',(1.,0.,0.));
#5151=DIRECTION('center_axis',(-0.74910748265946,0.,0.662448473032889));
#5152=DIRECTION('ref_axis',(-0.662448473032889,1.76182853028895E-15,-0.74910748265946));
#5153=DIRECTION('center_axis',(0.,1.,0.));
#5154=DIRECTION('ref_axis',(1.,0.,0.));
#5155=DIRECTION('center_axis',(-1.95250156806324E-14,-0.287196439203363,
0.957871706080156));
#5156=DIRECTION('ref_axis',(-4.61450960908913E-30,0.957871706080156,0.287196439203363));
#5157=DIRECTION('center_axis',(-1.,0.,0.));
#5158=DIRECTION('ref_axis',(0.,0.,1.));
#5159=DIRECTION('center_axis',(-5.33981346144544E-14,-0.101086417024396,
-0.994877648906221));
#5160=DIRECTION('ref_axis',(1.35459394958056E-29,0.994877648906221,-0.101086417024396));
#5161=DIRECTION('center_axis',(0.,1.,0.));
#5162=DIRECTION('ref_axis',(0.,0.,1.));
#5163=DIRECTION('center_axis',(-0.199143465014975,0.,-0.979970346664546));
#5164=DIRECTION('ref_axis',(-0.979970346664546,0.,0.199143465014975));
#5165=DIRECTION('center_axis',(0.,1.,0.));
#5166=DIRECTION('ref_axis',(0.,0.,1.));
#5167=DIRECTION('center_axis',(-0.199143465014928,4.4226733372247E-14,0.979970346664555));
#5168=DIRECTION('ref_axis',(0.979970346664555,-4.97863136211578E-29,0.199143465014928));
#5169=DIRECTION('center_axis',(-1.,0.,0.));
#5170=DIRECTION('ref_axis',(0.,0.,1.));
#5171=DIRECTION('center_axis',(0.,-0.101086417024344,0.994877648906226));
#5172=DIRECTION('ref_axis',(0.,-0.994877648906226,-0.101086417024344));
#5173=DIRECTION('center_axis',(0.,1.,0.));
#5174=DIRECTION('ref_axis',(1.,0.,0.));
#5175=DIRECTION('center_axis',(0.,1.14925430283463E-13,-1.));
#5176=DIRECTION('ref_axis',(0.,-1.,-1.14925430283463E-13));
#5177=DIRECTION('center_axis',(0.,1.,0.));
#5178=DIRECTION('ref_axis',(-0.994979986397858,0.,-0.100074105880182));
#5179=DIRECTION('center_axis',(-1.14925430283463E-13,0.,1.));
#5180=DIRECTION('ref_axis',(-1.,0.,-1.14925430283463E-13));
#5181=DIRECTION('center_axis',(0.,0.,1.));
#5182=DIRECTION('ref_axis',(1.,0.,0.));
#5183=DIRECTION('center_axis',(0.,-1.,0.));
#5184=DIRECTION('ref_axis',(0.,0.,-1.));
#5185=DIRECTION('axis',(0.,0.,1.));
#5186=DIRECTION('refdir',(1.,0.,0.));
#5187=DIRECTION('center_axis',(0.,-1.,0.));
#5188=DIRECTION('ref_axis',(0.,0.,-1.));
#5189=DIRECTION('center_axis',(-1.,0.,-1.22464679914735E-16));
#5190=DIRECTION('ref_axis',(-1.22464679914735E-16,0.,1.));
#5191=DIRECTION('center_axis',(0.,1.,0.));
#5192=DIRECTION('ref_axis',(0.,0.,-1.));
#5193=DIRECTION('axis',(0.,0.,1.));
#5194=DIRECTION('refdir',(1.,0.,0.));
#5195=DIRECTION('center_axis',(0.,-1.,0.));
#5196=DIRECTION('ref_axis',(0.,0.,-1.));
#5197=DIRECTION('center_axis',(-1.,0.,-1.22464679914735E-16));
#5198=DIRECTION('ref_axis',(-1.22464679914735E-16,0.,1.));
#5199=DIRECTION('center_axis',(0.,1.,0.));
#5200=DIRECTION('ref_axis',(0.,0.,-1.));
#5201=DIRECTION('center_axis',(0.,-1.,0.));
#5202=DIRECTION('ref_axis',(0.,0.,-1.));
#5203=DIRECTION('center_axis',(-1.,0.,-1.22464679914735E-16));
#5204=DIRECTION('ref_axis',(-1.22464679914735E-16,0.,1.));
#5205=DIRECTION('center_axis',(0.,1.,0.));
#5206=DIRECTION('ref_axis',(0.,0.,-1.));
#5207=DIRECTION('center_axis',(0.715813339017001,0.0683962349942489,-0.694933967168064));
#5208=DIRECTION('ref_axis',(0.0832680595661294,0.979730076642959,0.182196067952284));
#5209=DIRECTION('center_axis',(0.721009996323288,0.136469090742821,-0.679353201562869));
#5210=DIRECTION('ref_axis',(-0.685769030757116,2.74420183243792E-16,-0.727819233363921));
#5211=DIRECTION('center_axis',(0.721009996323288,0.136469090742821,-0.679353201562869));
#5212=DIRECTION('ref_axis',(-0.685769030757116,2.74420183243792E-16,-0.727819233363921));
#5213=DIRECTION('center_axis',(0.721009996323288,0.136469090742821,-0.679353201562869));
#5214=DIRECTION('ref_axis',(-0.685769030757116,9.43576066543432E-18,-0.727819233363921));
#5215=DIRECTION('',(0.,0.,1.));
#5216=DIRECTION('',(1.,0.,0.));
#5217=DIRECTION('',(-2.22618990321803E-16,1.11022302462516E-16,-1.));
#5218=DIRECTION('',(-1.,-2.16993472821069E-16,2.22618990321803E-16));
#5219=DIRECTION('',(2.35055030994857E-16,-0.0143876041762839,0.999896493066191));
#5220=DIRECTION('',(1.,1.50993216358444E-16,-2.32906707823779E-16));
#5221=DIRECTION('',(-1.,-3.54226952870771E-16,7.4433150696658E-17));
#5222=DIRECTION('',(7.4433150696658E-17,-2.77555756156289E-17,1.));
#5223=DIRECTION('',(0.,0.,1.));
#5224=DIRECTION('',(1.,0.,0.));
#5225=DIRECTION('',(-1.,4.57710679677258E-17,0.));
#5226=DIRECTION('',(2.09499066290617E-33,4.57710679677258E-17,1.));
#5227=DIRECTION('',(0.,0.,1.));
#5228=DIRECTION('',(1.83084271870903E-16,-1.,0.));
#5229=DIRECTION('',(0.,0.,1.));
#5230=DIRECTION('',(1.83084271870903E-16,-1.,0.));
#5231=DIRECTION('',(1.36611743369565E-16,-0.735334110295695,-0.677704763326656));
#5232=DIRECTION('',(2.14856461581709E-16,-0.677704763326656,0.735334110295695));
#5233=CARTESIAN_POINT('',(0.,0.,0.));
#5234=CARTESIAN_POINT('',(0.,0.,0.));
#5235=CARTESIAN_POINT('Origin',(7.50000000000001,0.,-7.751));
#5236=CARTESIAN_POINT('',(6.275,-1.50019232895551E-16,6.54999999999999));
#5237=CARTESIAN_POINT('Origin',(7.50000000000001,0.,6.54999999999999));
#5238=CARTESIAN_POINT('',(6.275,-1.50019232895551E-16,7.75));
#5239=CARTESIAN_POINT('',(6.275,-1.50019232895551E-16,-7.751));
#5240=CARTESIAN_POINT('Origin',(7.50000000000001,0.,7.75));
#5241=CARTESIAN_POINT('Origin',(-7.5,0.,-7.751));
#5242=CARTESIAN_POINT('',(-8.725,-1.50019232895551E-16,6.55));
#5243=CARTESIAN_POINT('Origin',(-7.5,0.,6.55));
#5244=CARTESIAN_POINT('',(-8.725,-1.50019232895551E-16,7.75));
#5245=CARTESIAN_POINT('',(-8.725,-1.50019232895551E-16,-7.751));
#5246=CARTESIAN_POINT('Origin',(-7.5,0.,7.75));
#5247=CARTESIAN_POINT('Origin',(-15.001,0.,3.35775314362943E-15));
#5248=CARTESIAN_POINT('',(13.8,-2.02066721859313E-16,1.65));
#5249=CARTESIAN_POINT('Origin',(13.8,0.,-3.08892696367483E-15));
#5250=CARTESIAN_POINT('',(15.,-2.02066721859313E-16,1.65));
#5251=CARTESIAN_POINT('',(-15.001,-2.02066721859313E-16,1.65));
#5252=CARTESIAN_POINT('Origin',(15.,0.,-3.35752930834221E-15));
#5253=CARTESIAN_POINT('Origin',(-15.,6.75,-7.75));
#5254=CARTESIAN_POINT('',(-15.,6.75,-7.75));
#5255=CARTESIAN_POINT('',(-15.,2.775,-7.75));
#5256=CARTESIAN_POINT('',(-15.,6.75,-7.75));
#5257=CARTESIAN_POINT('',(-15.,2.775,-6.55));
#5258=CARTESIAN_POINT('',(-15.,2.775,-7.75));
#5259=CARTESIAN_POINT('',(-15.,6.75,-6.55));
#5260=CARTESIAN_POINT('',(-15.,-6.75,-6.55));
#5261=CARTESIAN_POINT('',(-15.,6.75,-7.75));
#5262=CARTESIAN_POINT('Origin',(-15.,6.75,-7.75));
#5263=CARTESIAN_POINT('',(-15.,2.775,6.55));
#5264=CARTESIAN_POINT('',(-15.,6.75,6.55));
#5265=CARTESIAN_POINT('',(-15.,-6.75,6.55));
#5266=CARTESIAN_POINT('',(-15.,2.775,7.75));
#5267=CARTESIAN_POINT('',(-15.,2.775,-7.75));
#5268=CARTESIAN_POINT('',(-15.,6.75,7.75));
#5269=CARTESIAN_POINT('',(-15.,6.75,7.75));
#5270=CARTESIAN_POINT('',(-15.,6.75,-7.75));
#5271=CARTESIAN_POINT('Origin',(-15.,6.75,-7.75));
#5272=CARTESIAN_POINT('',(-15.,-6.75,-6.55));
#5273=CARTESIAN_POINT('',(-15.,-2.775,-6.55));
#5274=CARTESIAN_POINT('',(-15.,-6.75,-6.55));
#5275=CARTESIAN_POINT('',(-15.,-2.775,-7.75));
#5276=CARTESIAN_POINT('',(-15.,-2.775,-7.75));
#5277=CARTESIAN_POINT('',(-15.,-6.75,-7.75));
#5278=CARTESIAN_POINT('',(-15.,6.75,-7.75));
#5279=CARTESIAN_POINT('',(-15.,-6.75,-7.75));
#5280=CARTESIAN_POINT('Origin',(-15.,6.75,-7.75));
#5281=CARTESIAN_POINT('',(-15.,-2.775,7.75));
#5282=CARTESIAN_POINT('',(-15.,-6.75,7.75));
#5283=CARTESIAN_POINT('',(-15.,6.75,7.75));
#5284=CARTESIAN_POINT('',(-15.,-2.775,6.55));
#5285=CARTESIAN_POINT('',(-15.,-2.775,-7.75));
#5286=CARTESIAN_POINT('',(-15.,-6.75,6.55));
#5287=CARTESIAN_POINT('',(-15.,-6.75,6.55));
#5288=CARTESIAN_POINT('',(-15.,-6.75,-7.75));
#5289=CARTESIAN_POINT('Origin',(-15.,6.75,7.75));
#5290=CARTESIAN_POINT('',(-13.,2.775,7.75));
#5291=CARTESIAN_POINT('',(-15.,2.775,7.75));
#5292=CARTESIAN_POINT('',(-13.,-2.775,7.75));
#5293=CARTESIAN_POINT('',(-13.,2.775,7.75));
#5294=CARTESIAN_POINT('',(-15.,-2.775,7.75));
#5295=CARTESIAN_POINT('',(14.,-6.75,7.75));
#5296=CARTESIAN_POINT('',(-15.,-6.75,7.75));
#5297=CARTESIAN_POINT('',(14.,6.75,7.75));
#5298=CARTESIAN_POINT('',(14.,6.75,7.75));
#5299=CARTESIAN_POINT('',(-15.,6.75,7.75));
#5300=CARTESIAN_POINT('Origin',(15.,6.75,-7.75));
#5301=CARTESIAN_POINT('',(15.,6.75,6.75));
#5302=CARTESIAN_POINT('',(15.,6.75,-6.75));
#5303=CARTESIAN_POINT('',(15.,6.75,-7.75));
#5304=CARTESIAN_POINT('',(15.,-6.75,6.75));
#5305=CARTESIAN_POINT('',(15.,6.75,6.75));
#5306=CARTESIAN_POINT('',(15.,-6.75,-6.75));
#5307=CARTESIAN_POINT('',(15.,-6.75,-7.75));
#5308=CARTESIAN_POINT('',(15.,6.75,-6.75));
#5309=CARTESIAN_POINT('Origin',(-15.,6.75,-7.75));
#5310=CARTESIAN_POINT('',(-13.,-2.775,-7.75));
#5311=CARTESIAN_POINT('',(-13.,2.775,-7.75));
#5312=CARTESIAN_POINT('',(-13.,2.775,-7.75));
#5313=CARTESIAN_POINT('',(-15.,2.775,-7.75));
#5314=CARTESIAN_POINT('',(14.,6.75,-7.75));
#5315=CARTESIAN_POINT('',(-15.,6.75,-7.75));
#5316=CARTESIAN_POINT('',(14.,-6.75,-7.75));
#5317=CARTESIAN_POINT('',(14.,6.75,-7.75));
#5318=CARTESIAN_POINT('',(-15.,-6.75,-7.75));
#5319=CARTESIAN_POINT('',(-15.,-2.775,-7.75));
#5320=CARTESIAN_POINT('Origin',(0.,6.75,0.));
#5321=CARTESIAN_POINT('Origin',(14.,6.75,6.75));
#5322=CARTESIAN_POINT('Origin',(14.,6.75,-6.75));
#5323=CARTESIAN_POINT('',(13.6,6.75,-6.55));
#5324=CARTESIAN_POINT('',(-15.,6.75,-6.55));
#5325=CARTESIAN_POINT('',(13.8,6.75,-6.35));
#5326=CARTESIAN_POINT('Origin',(13.6,6.75,-6.35));
#5327=CARTESIAN_POINT('',(13.8,6.75,6.34999999999999));
#5328=CARTESIAN_POINT('',(13.8,6.75,6.54999999999999));
#5329=CARTESIAN_POINT('',(13.6,6.75,6.54999999999999));
#5330=CARTESIAN_POINT('Origin',(13.6,6.75,6.34999999999999));
#5331=CARTESIAN_POINT('',(-15.,6.75,6.55));
#5332=CARTESIAN_POINT('Origin',(0.,-6.75,0.));
#5333=CARTESIAN_POINT('Origin',(14.,-6.75,6.75));
#5334=CARTESIAN_POINT('',(13.6,-6.75,6.54999999999999));
#5335=CARTESIAN_POINT('',(-15.,-6.75,6.55));
#5336=CARTESIAN_POINT('',(13.8,-6.75,6.34999999999999));
#5337=CARTESIAN_POINT('Origin',(13.6,-6.75,6.34999999999999));
#5338=CARTESIAN_POINT('',(13.8,-6.75,-6.35));
#5339=CARTESIAN_POINT('',(13.8,-6.75,6.54999999999999));
#5340=CARTESIAN_POINT('',(13.6,-6.75,-6.55));
#5341=CARTESIAN_POINT('Origin',(13.6,-6.75,-6.35));
#5342=CARTESIAN_POINT('',(-15.,-6.75,-6.55));
#5343=CARTESIAN_POINT('Origin',(14.,-6.75,-6.75));
#5344=CARTESIAN_POINT('Origin',(-15.,-6.75,-6.55));
#5345=CARTESIAN_POINT('',(-13.,2.775,-6.55));
#5346=CARTESIAN_POINT('',(-15.,2.775,-6.55));
#5347=CARTESIAN_POINT('',(-13.,-2.775,-6.55));
#5348=CARTESIAN_POINT('',(-13.,-6.75,-6.55));
#5349=CARTESIAN_POINT('',(-15.,-2.775,-6.55));
#5350=CARTESIAN_POINT('',(13.6,6.75,-6.55));
#5351=CARTESIAN_POINT('Origin',(13.8,-6.75,6.54999999999999));
#5352=CARTESIAN_POINT('',(13.8,6.75,6.34999999999999));
#5353=CARTESIAN_POINT('',(13.8,-6.75,-6.35));
#5354=CARTESIAN_POINT('Origin',(-15.,-6.75,6.55));
#5355=CARTESIAN_POINT('',(-13.,-2.775,6.55));
#5356=CARTESIAN_POINT('',(-13.,2.775,6.55));
#5357=CARTESIAN_POINT('',(-13.,-6.75,6.55));
#5358=CARTESIAN_POINT('',(-15.,2.775,6.55));
#5359=CARTESIAN_POINT('',(13.6,-6.75,6.54999999999999));
#5360=CARTESIAN_POINT('',(-15.,-2.775,6.55));
#5361=CARTESIAN_POINT('Origin',(14.,6.75,6.75));
#5362=CARTESIAN_POINT('Origin',(14.,6.75,-6.75));
#5363=CARTESIAN_POINT('Origin',(13.6,-6.75,6.34999999999999));
#5364=CARTESIAN_POINT('Origin',(13.6,-6.75,-6.35));
#5365=CARTESIAN_POINT('Origin',(-15.,-2.775,-7.75));
#5366=CARTESIAN_POINT('',(-13.,-2.775,-7.75));
#5367=CARTESIAN_POINT('Origin',(-13.,2.775,-7.75));
#5368=CARTESIAN_POINT('',(-13.,2.775,-7.75));
#5369=CARTESIAN_POINT('Origin',(-15.,2.775,-7.75));
#5370=CARTESIAN_POINT('Origin',(-15.,2.775,-7.75));
#5371=CARTESIAN_POINT('',(-13.,2.775,-7.75));
#5372=CARTESIAN_POINT('Origin',(-13.,2.775,-7.75));
#5373=CARTESIAN_POINT('',(-13.,-2.775,-7.75));
#5374=CARTESIAN_POINT('Origin',(-15.,-2.775,-7.75));
#5375=CARTESIAN_POINT('',(0.,0.,0.));
#5376=CARTESIAN_POINT('Origin',(-14.001,-1.85863229568951E-19,0.));
#5377=CARTESIAN_POINT('',(-14.,-3.075,-3.76578890737811E-16));
#5378=CARTESIAN_POINT('Origin',(-14.,5.01301320851673E-31,0.));
#5379=CARTESIAN_POINT('',(14.,-3.075,-3.76578890737811E-16));
#5380=CARTESIAN_POINT('',(-14.001,-3.075,-3.76578890737811E-16));
#5381=CARTESIAN_POINT('Origin',(14.,5.20417042793042E-15,0.));
#5382=CARTESIAN_POINT('Origin',(-14.,0.,0.));
#5383=CARTESIAN_POINT('',(-13.,4.1,-5.02105187650415E-16));
#5384=CARTESIAN_POINT('Origin',(-13.,1.85863229568944E-16,0.));
#5385=CARTESIAN_POINT('',(11.8,4.1,-5.02105187650415E-16));
#5386=CARTESIAN_POINT('',(-14.,4.1,-5.02105187650415E-16));
#5387=CARTESIAN_POINT('Origin',(11.8,4.79527132287875E-15,0.));
#5388=CARTESIAN_POINT('Origin',(-14.,0.,0.));
#5389=CARTESIAN_POINT('',(12.8,4.1,-5.02105187650415E-16));
#5390=CARTESIAN_POINT('Origin',(12.8,4.98113455244769E-15,0.));
#5391=CARTESIAN_POINT('',(14.,4.1,-5.02105187650415E-16));
#5392=CARTESIAN_POINT('',(-14.,4.1,-5.02105187650415E-16));
#5393=CARTESIAN_POINT('Origin',(14.,5.20417042793042E-15,0.));
#5394=CARTESIAN_POINT('Origin',(14.,5.20417042793042E-15,0.));
#5395=CARTESIAN_POINT('Origin',(12.8,6.5,6.));
#5396=CARTESIAN_POINT('',(11.8,6.,6.));
#5397=CARTESIAN_POINT('',(11.8,-5.99999999999999,6.));
#5398=CARTESIAN_POINT('',(11.8,6.5,6.));
#5399=CARTESIAN_POINT('',(12.8,-5.99999999999999,6.));
#5400=CARTESIAN_POINT('',(12.8,-6.,6.));
#5401=CARTESIAN_POINT('',(12.8,6.,6.));
#5402=CARTESIAN_POINT('',(12.8,6.5,6.));
#5403=CARTESIAN_POINT('',(12.8,6.,6.));
#5404=CARTESIAN_POINT('Origin',(12.8,-6.5,6.));
#5405=CARTESIAN_POINT('',(11.8,-6.5,5.5));
#5406=CARTESIAN_POINT('',(11.8,-6.5,-5.5));
#5407=CARTESIAN_POINT('',(11.8,-6.5,6.));
#5408=CARTESIAN_POINT('',(12.8,-6.5,-5.5));
#5409=CARTESIAN_POINT('',(12.8,-6.5,-5.5));
#5410=CARTESIAN_POINT('',(12.8,-6.5,5.5));
#5411=CARTESIAN_POINT('',(12.8,-6.5,6.));
#5412=CARTESIAN_POINT('',(12.8,-6.5,5.5));
#5413=CARTESIAN_POINT('Origin',(12.8,6.5,-6.));
#5414=CARTESIAN_POINT('',(12.8,-5.99999999999999,-6.));
#5415=CARTESIAN_POINT('',(12.8,6.,-6.));
#5416=CARTESIAN_POINT('',(12.8,6.5,-6.));
#5417=CARTESIAN_POINT('',(11.8,-5.99999999999999,-6.));
#5418=CARTESIAN_POINT('',(12.8,-6.,-6.));
#5419=CARTESIAN_POINT('',(11.8,6.,-6.));
#5420=CARTESIAN_POINT('',(11.8,6.5,-6.));
#5421=CARTESIAN_POINT('',(12.8,6.,-6.));
#5422=CARTESIAN_POINT('Origin',(12.8,6.5,6.));
#5423=CARTESIAN_POINT('',(12.8,6.5,-5.5));
#5424=CARTESIAN_POINT('',(12.8,6.5,5.5));
#5425=CARTESIAN_POINT('',(12.8,6.5,6.));
#5426=CARTESIAN_POINT('',(11.8,6.5,-5.5));
#5427=CARTESIAN_POINT('',(12.8,6.5,-5.5));
#5428=CARTESIAN_POINT('',(11.8,6.5,5.5));
#5429=CARTESIAN_POINT('',(11.8,6.5,6.));
#5430=CARTESIAN_POINT('',(12.8,6.5,5.5));
#5431=CARTESIAN_POINT('Origin',(12.8,3.33505353980376E-15,0.));
#5432=CARTESIAN_POINT('Origin',(12.8,-6.,-5.5));
#5433=CARTESIAN_POINT('Origin',(12.8,6.,-5.5));
#5434=CARTESIAN_POINT('Origin',(12.8,6.,5.5));
#5435=CARTESIAN_POINT('Origin',(12.8,-6.,5.5));
#5436=CARTESIAN_POINT('Origin',(11.8,3.14919031023482E-15,0.));
#5437=CARTESIAN_POINT('Origin',(11.8,-6.,-5.5));
#5438=CARTESIAN_POINT('Origin',(11.8,-6.,5.5));
#5439=CARTESIAN_POINT('Origin',(11.8,6.,5.5));
#5440=CARTESIAN_POINT('Origin',(11.8,6.,-5.5));
#5441=CARTESIAN_POINT('Origin',(-13.,-6.5,-6.));
#5442=CARTESIAN_POINT('',(-13.,5.99999999999999,-6.));
#5443=CARTESIAN_POINT('',(-13.,-6.,-6.));
#5444=CARTESIAN_POINT('',(-13.,-6.5,-6.));
#5445=CARTESIAN_POINT('',(-14.,-6.,-6.));
#5446=CARTESIAN_POINT('',(-13.,-6.,-6.));
#5447=CARTESIAN_POINT('',(-14.,5.99999999999999,-6.));
#5448=CARTESIAN_POINT('',(-14.,-6.5,-6.));
#5449=CARTESIAN_POINT('',(-13.,6.,-6.));
#5450=CARTESIAN_POINT('Origin',(-13.,6.5,-6.));
#5451=CARTESIAN_POINT('',(-13.,6.5,5.5));
#5452=CARTESIAN_POINT('',(-13.,6.5,-5.5));
#5453=CARTESIAN_POINT('',(-13.,6.5,-6.));
#5454=CARTESIAN_POINT('',(-14.,6.5,-5.5));
#5455=CARTESIAN_POINT('',(-13.,6.5,-5.5));
#5456=CARTESIAN_POINT('',(-14.,6.5,5.5));
#5457=CARTESIAN_POINT('',(-14.,6.5,-6.));
#5458=CARTESIAN_POINT('',(-13.,6.5,5.5));
#5459=CARTESIAN_POINT('Origin',(-13.,6.5,6.));
#5460=CARTESIAN_POINT('',(-14.,-6.,6.));
#5461=CARTESIAN_POINT('',(-14.,6.,6.));
#5462=CARTESIAN_POINT('',(-14.,6.5,6.));
#5463=CARTESIAN_POINT('',(-13.,-6.,6.));
#5464=CARTESIAN_POINT('',(-13.,-6.,6.));
#5465=CARTESIAN_POINT('',(-13.,6.,6.));
#5466=CARTESIAN_POINT('',(-13.,6.5,6.));
#5467=CARTESIAN_POINT('',(-13.,6.,6.));
#5468=CARTESIAN_POINT('Origin',(-13.,-6.5,6.));
#5469=CARTESIAN_POINT('',(-14.,-6.5,-5.5));
#5470=CARTESIAN_POINT('',(-14.,-6.5,5.5));
#5471=CARTESIAN_POINT('',(-14.,-6.5,6.));
#5472=CARTESIAN_POINT('',(-13.,-6.5,-5.5));
#5473=CARTESIAN_POINT('',(-13.,-6.5,-5.5));
#5474=CARTESIAN_POINT('',(-13.,-6.5,5.5));
#5475=CARTESIAN_POINT('',(-13.,-6.5,6.));
#5476=CARTESIAN_POINT('',(-13.,-6.5,5.5));
#5477=CARTESIAN_POINT('Origin',(-13.,-3.55046425715033E-15,0.));
#5478=CARTESIAN_POINT('Origin',(-13.,-6.,-5.5));
#5479=CARTESIAN_POINT('Origin',(-13.,6.,-5.5));
#5480=CARTESIAN_POINT('Origin',(-13.,6.,5.5));
#5481=CARTESIAN_POINT('Origin',(-13.,-6.,5.5));
#5482=CARTESIAN_POINT('Origin',(-14.,7.08175372168856E-32,0.));
#5483=CARTESIAN_POINT('Origin',(-14.,-6.,-5.5));
#5484=CARTESIAN_POINT('Origin',(-14.,-6.,5.5));
#5485=CARTESIAN_POINT('Origin',(-14.,6.,5.5));
#5486=CARTESIAN_POINT('Origin',(-14.,6.,-5.5));
#5487=CARTESIAN_POINT('Origin',(-13.,-6.,-5.5));
#5488=CARTESIAN_POINT('Origin',(-13.,-6.,5.5));
#5489=CARTESIAN_POINT('Origin',(-13.,6.,-5.5));
#5490=CARTESIAN_POINT('Origin',(-13.,6.,5.5));
#5491=CARTESIAN_POINT('Origin',(12.8,-6.,-5.5));
#5492=CARTESIAN_POINT('Origin',(12.8,-6.,5.5));
#5493=CARTESIAN_POINT('Origin',(12.8,6.,-5.5));
#5494=CARTESIAN_POINT('Origin',(12.8,6.,5.5));
#5495=CARTESIAN_POINT('',(0.,0.,0.));
#5496=CARTESIAN_POINT('Origin',(-12.4,0.,0.));
#5497=CARTESIAN_POINT('',(-12.4,-7.71527483462833E-16,-6.3));
#5498=CARTESIAN_POINT('Origin',(-12.4,0.,0.));
#5499=CARTESIAN_POINT('',(12.4,-7.71527483462833E-16,-6.3));
#5500=CARTESIAN_POINT('',(-12.4,-7.71527483462833E-16,-6.3));
#5501=CARTESIAN_POINT('Origin',(12.4,0.,0.));
#5502=CARTESIAN_POINT('Origin',(-12.4,0.,0.));
#5503=CARTESIAN_POINT('',(12.4,-5.02105187650415E-16,-4.1));
#5504=CARTESIAN_POINT('Origin',(12.4,0.,0.));
#5505=CARTESIAN_POINT('',(-12.4,-5.02105187650415E-16,-4.1));
#5506=CARTESIAN_POINT('',(-12.4,-5.02105187650415E-16,-4.1));
#5507=CARTESIAN_POINT('Origin',(-12.4,0.,0.));
#5508=CARTESIAN_POINT('Origin',(-12.4,6.3,0.));
#5509=CARTESIAN_POINT('Origin',(12.4,6.3,0.));
#5510=CARTESIAN_POINT('',(0.,0.,0.));
#5511=CARTESIAN_POINT('Origin',(0.,0.,-0.000999999999999916));
#5512=CARTESIAN_POINT('',(-4.2,-5.14351655641888E-16,0.));
#5513=CARTESIAN_POINT('Origin',(0.,0.,0.));
#5514=CARTESIAN_POINT('',(-4.2,-5.14351655641888E-16,1.2));
#5515=CARTESIAN_POINT('',(-4.2,-5.14351655641888E-16,-0.000999999999999916));
#5516=CARTESIAN_POINT('Origin',(0.,0.,1.2));
#5517=CARTESIAN_POINT('Origin',(-7.5,6.5,1.2));
#5518=CARTESIAN_POINT('',(-7.5,2.775,1.2));
#5519=CARTESIAN_POINT('',(-7.5,-2.775,1.2));
#5520=CARTESIAN_POINT('',(-7.5,6.5,1.2));
#5521=CARTESIAN_POINT('',(-7.5,2.775,0.));
#5522=CARTESIAN_POINT('',(-7.5,2.775,-0.000999999999999916));
#5523=CARTESIAN_POINT('',(-7.5,-2.775,0.));
#5524=CARTESIAN_POINT('',(-7.5,6.5,0.));
#5525=CARTESIAN_POINT('',(-7.5,-2.775,-0.000999999999999916));
#5526=CARTESIAN_POINT('Origin',(-7.5,-6.5,1.2));
#5527=CARTESIAN_POINT('',(-6.55,-6.5,1.2));
#5528=CARTESIAN_POINT('',(6.55,-6.5,1.2));
#5529=CARTESIAN_POINT('',(-7.5,-6.5,1.2));
#5530=CARTESIAN_POINT('',(-6.55,-6.5,0.));
#5531=CARTESIAN_POINT('',(-6.55,-6.5,-0.000999999999999916));
#5532=CARTESIAN_POINT('',(6.55,-6.5,0.));
#5533=CARTESIAN_POINT('',(-7.5,-6.5,0.));
#5534=CARTESIAN_POINT('',(6.55,-6.5,-0.000999999999999916));
#5535=CARTESIAN_POINT('Origin',(7.5,6.5,1.2));
#5536=CARTESIAN_POINT('',(7.5,-2.775,1.2));
#5537=CARTESIAN_POINT('',(7.5,2.775,1.2));
#5538=CARTESIAN_POINT('',(7.5,6.5,1.2));
#5539=CARTESIAN_POINT('',(7.5,-2.775,0.));
#5540=CARTESIAN_POINT('',(7.5,-2.775,-0.000999999999999916));
#5541=CARTESIAN_POINT('',(7.5,2.775,0.));
#5542=CARTESIAN_POINT('',(7.5,6.5,0.));
#5543=CARTESIAN_POINT('',(7.5,2.775,-0.000999999999999916));
#5544=CARTESIAN_POINT('Origin',(-7.5,6.5,1.2));
#5545=CARTESIAN_POINT('',(6.55,6.5,0.));
#5546=CARTESIAN_POINT('',(-6.55,6.5,0.));
#5547=CARTESIAN_POINT('',(-7.5,6.5,0.));
#5548=CARTESIAN_POINT('',(-6.55,6.5,1.2));
#5549=CARTESIAN_POINT('',(-6.55,6.5,-0.000999999999999916));
#5550=CARTESIAN_POINT('',(6.55,6.5,1.2));
#5551=CARTESIAN_POINT('',(-7.5,6.5,1.2));
#5552=CARTESIAN_POINT('',(6.55,6.5,-0.000999999999999916));
#5553=CARTESIAN_POINT('Origin',(0.,0.,1.2));
#5554=CARTESIAN_POINT('',(-6.55,2.775,1.2));
#5555=CARTESIAN_POINT('',(-6.55,6.5,1.2));
#5556=CARTESIAN_POINT('',(-7.5,2.775,1.2));
#5557=CARTESIAN_POINT('',(-6.55,-2.775,1.2));
#5558=CARTESIAN_POINT('',(-7.5,-2.775,1.2));
#5559=CARTESIAN_POINT('',(-6.55,-6.5,1.2));
#5560=CARTESIAN_POINT('',(6.55,-2.775,1.2));
#5561=CARTESIAN_POINT('',(6.55,-6.5,1.2));
#5562=CARTESIAN_POINT('',(7.5,-2.775,1.2));
#5563=CARTESIAN_POINT('',(6.55,2.775,1.2));
#5564=CARTESIAN_POINT('',(7.5,2.775,1.2));
#5565=CARTESIAN_POINT('',(6.55,6.5,1.2));
#5566=CARTESIAN_POINT('Origin',(0.,0.,0.));
#5567=CARTESIAN_POINT('',(-6.55,2.775,0.));
#5568=CARTESIAN_POINT('',(-7.5,2.775,0.));
#5569=CARTESIAN_POINT('',(-6.55,6.5,0.));
#5570=CARTESIAN_POINT('',(6.55,2.775,0.));
#5571=CARTESIAN_POINT('',(6.55,6.5,0.));
#5572=CARTESIAN_POINT('',(7.5,2.775,0.));
#5573=CARTESIAN_POINT('',(6.55,-2.775,0.));
#5574=CARTESIAN_POINT('',(7.5,-2.775,0.));
#5575=CARTESIAN_POINT('',(6.55,-6.5,0.));
#5576=CARTESIAN_POINT('',(-6.55,-2.775,0.));
#5577=CARTESIAN_POINT('',(-6.55,-6.5,0.));
#5578=CARTESIAN_POINT('',(-7.5,-2.775,0.));
#5579=CARTESIAN_POINT('Origin',(7.5,2.775,-0.000999999999999916));
#5580=CARTESIAN_POINT('',(6.55,2.775,-0.000999999999999916));
#5581=CARTESIAN_POINT('Origin',(6.55,6.5,-0.000999999999999916));
#5582=CARTESIAN_POINT('Origin',(6.55,-6.5,-0.000999999999999916));
#5583=CARTESIAN_POINT('',(6.55,-2.775,-0.000999999999999916));
#5584=CARTESIAN_POINT('Origin',(7.5,-2.775,-0.000999999999999916));
#5585=CARTESIAN_POINT('Origin',(-7.5,-2.775,-0.000999999999999916));
#5586=CARTESIAN_POINT('',(-6.55,-2.775,-0.000999999999999916));
#5587=CARTESIAN_POINT('Origin',(-6.55,-6.5,-0.000999999999999916));
#5588=CARTESIAN_POINT('Origin',(-6.55,6.5,-0.000999999999999916));
#5589=CARTESIAN_POINT('',(-6.55,2.775,-0.000999999999999916));
#5590=CARTESIAN_POINT('Origin',(-7.5,2.775,-0.000999999999999916));
#5591=CARTESIAN_POINT('',(0.,0.,0.));
#5592=CARTESIAN_POINT('Ctrl Pts',(-24.7512205732181,1.27647900817359E-15,
-3.00000039251396));
#5593=CARTESIAN_POINT('Ctrl Pts',(-24.7512209918384,0.0224904489448925,
-3.0000001742556));
#5594=CARTESIAN_POINT('Ctrl Pts',(-24.7517089574441,0.0449130845232472,
-2.99974733834206));
#5595=CARTESIAN_POINT('Ctrl Pts',(-24.7536443519837,0.0895752381506401,
-2.99874599882651));
#5596=CARTESIAN_POINT('Ctrl Pts',(-24.7550914179306,0.111823200513364,-2.9979976955573));
#5597=CARTESIAN_POINT('Ctrl Pts',(-24.7608544959128,0.178320919528196,-2.99502476849759));
#5598=CARTESIAN_POINT('Ctrl Pts',(-24.766591932863,0.222335186723984,-2.99207096785045));
#5599=CARTESIAN_POINT('Ctrl Pts',(-24.7780291872986,0.28783719851668,-2.98624078109656));
#5600=CARTESIAN_POINT('Ctrl Pts',(-24.7823200974485,0.309606387247319,-2.98406110217343));
#5601=CARTESIAN_POINT('Ctrl Pts',(-24.789468342319,0.342109605994458,-2.98045008409494));
#5602=CARTESIAN_POINT('Ctrl Pts',(-24.7919728029526,0.352929856681449,-2.97918798270958));
#5603=CARTESIAN_POINT('Ctrl Pts',(-24.7972217651647,0.374523130101453,-2.97655057002885));
#5604=CARTESIAN_POINT('Ctrl Pts',(-24.7999685317995,0.3853026801014,-2.97517414639763));
#5605=CARTESIAN_POINT('Ctrl Pts',(-24.8085250872429,0.417396090242857,-2.97090016875934));
#5606=CARTESIAN_POINT('Ctrl Pts',(-24.81466151752,0.438519418189055,-2.96785256118554));
#5607=CARTESIAN_POINT('Ctrl Pts',(-24.8277811472732,0.480245335622271,-2.96138693176614));
#5608=CARTESIAN_POINT('Ctrl Pts',(-24.8347637590013,0.500846703560909,-2.95796918269451));
#5609=CARTESIAN_POINT('Ctrl Pts',(-24.8569589172265,0.561884990270977,-2.94720128262928));
#5610=CARTESIAN_POINT('Ctrl Pts',(-24.8734161226417,0.601558077547724,-2.93933624108072));
#5611=CARTESIAN_POINT('Ctrl Pts',(-24.9005702937365,0.659577575494014,-2.92666224804854));
#5612=CARTESIAN_POINT('Ctrl Pts',(-24.9100346262345,0.678669948505798,-2.92229102401349));
#5613=CARTESIAN_POINT('Ctrl Pts',(-24.9297928233973,0.716355649282148,-2.91328208432799));
#5614=CARTESIAN_POINT('Ctrl Pts',(-24.9400945131254,0.734962441112191,-2.90864084409791));
#5615=CARTESIAN_POINT('Ctrl Pts',(-24.961514660095,0.771629674000388,-2.89912896911718));
#5616=CARTESIAN_POINT('Ctrl Pts',(-24.9725545674253,0.789557946478682,-2.89429319601545));
#5617=CARTESIAN_POINT('Ctrl Pts',(-24.9953084665056,0.824674949037349,-2.88448368582705));
#5618=CARTESIAN_POINT('Ctrl Pts',(-25.0070179507415,0.84185585681256,-2.87951192539658));
#5619=CARTESIAN_POINT('Ctrl Pts',(-25.043133571216,0.892292847196555,-2.86444548622589));
#5620=CARTESIAN_POINT('Ctrl Pts',(-25.0685243392037,0.924445728200641,-2.85419906644615));
#5621=CARTESIAN_POINT('Ctrl Pts',(-25.1085920152708,0.970518787083059,-2.83872479371572));
#5622=CARTESIAN_POINT('Ctrl Pts',(-25.1222787941031,0.985516398208715,-2.83354919922537));
#5623=CARTESIAN_POINT('Ctrl Pts',(-25.1503247573348,1.0147909893251,-2.82319728666854));
#5624=CARTESIAN_POINT('Ctrl Pts',(-25.164690788982,1.02907375849125,-2.81801865872126));
#5625=CARTESIAN_POINT('Ctrl Pts',(-25.1940841805899,1.05688925756545,-2.80770519124119));
#5626=CARTESIAN_POINT('Ctrl Pts',(-25.2091790647757,1.07047808243068,-2.80254833483865));
#5627=CARTESIAN_POINT('Ctrl Pts',(-25.2397860183817,1.09666813400314,-2.79240366726727));
#5628=CARTESIAN_POINT('Ctrl Pts',(-25.2553204379955,1.10929595959291,-2.78740689519964));
#5629=CARTESIAN_POINT('Ctrl Pts',(-25.2868471218303,1.13362876731756,-2.77759978805859));
#5630=CARTESIAN_POINT('Ctrl Pts',(-25.3028398226619,1.14533472511361,-2.77278915814534));
#5631=CARTESIAN_POINT('Ctrl Pts',(-25.3352862383422,1.16783527307202,-2.76338780408879));
#5632=CARTESIAN_POINT('Ctrl Pts',(-25.351739959153,1.17862983581217,-2.75879704618161));
#5633=CARTESIAN_POINT('Ctrl Pts',(-25.4018015943325,1.20964925021434,-2.74540688876098));
#5634=CARTESIAN_POINT('Ctrl Pts',(-25.4361159534219,1.22851653432306,-2.73698721829837));
#5635=CARTESIAN_POINT('Ctrl Pts',(-25.4890321005069,1.25402677583021,-2.72534532216722));
#5636=CARTESIAN_POINT('Ctrl Pts',(-25.5069295704027,1.26207047477093,-2.72162643380116));
#5637=CARTESIAN_POINT('Ctrl Pts',(-25.5341342320122,1.27341408145951,-2.71632781873948));
#5638=CARTESIAN_POINT('Ctrl Pts',(-25.5432728261675,1.27707857798257,-2.71460649012167));
#5639=CARTESIAN_POINT('Ctrl Pts',(-25.5616697300355,1.28416247287641,-2.71126260047886));
#5640=CARTESIAN_POINT('Ctrl Pts',(-25.5709428123064,1.28758661927442,-2.70963775628573));
#5641=CARTESIAN_POINT('Ctrl Pts',(-25.5987921995341,1.29743171221407,-2.70494481626589));
#5642=CARTESIAN_POINT('Ctrl Pts',(-25.6174339809943,1.30344290404711,-2.70205039524381));
#5643=CARTESIAN_POINT('Ctrl Pts',(-25.6548880488268,1.31438298806205,-2.69674565415259));
#5644=CARTESIAN_POINT('Ctrl Pts',(-25.6736969296858,1.31931098956043,-2.69433575157957));
#5645=CARTESIAN_POINT('Ctrl Pts',(-25.7303690862317,1.33248199267998,-2.68785983771893));
#5646=CARTESIAN_POINT('Ctrl Pts',(-25.7684774334826,1.33911568210638,-2.68454786410377));
#5647=CARTESIAN_POINT('Ctrl Pts',(-25.8261391530629,1.34582335222857,-2.6811878846237));
#5648=CARTESIAN_POINT('Ctrl Pts',(-25.8454430323917,1.34751786899547,-2.68033581181979));
#5649=CARTESIAN_POINT('Ctrl Pts',(-25.8842203925786,1.34980777647362,-2.67918335088873));
#5650=CARTESIAN_POINT('Ctrl Pts',(-25.903705143976,1.35040245497256,-2.67888335709824));
#5651=CARTESIAN_POINT('Ctrl Pts',(-25.9428031383705,1.3504709734195,-2.67884881443484));
#5652=CARTESIAN_POINT('Ctrl Pts',(-25.9625262668505,1.34993687451434,-2.67911827983487));
#5653=CARTESIAN_POINT('Ctrl Pts',(-26.0016751544635,1.34774181046255,-2.68022319148998));
#5654=CARTESIAN_POINT('Ctrl Pts',(-26.0211401155725,1.34608678179489,-2.68105562372842));
#5655=CARTESIAN_POINT('Ctrl Pts',(-26.059852112923,1.3416829898099,-2.68326212736971));
#5656=CARTESIAN_POINT('Ctrl Pts',(-26.0790998997345,1.33893483082381,-2.68463587910205));
#5657=CARTESIAN_POINT('Ctrl Pts',(-26.1173832113779,1.33236210276061,-2.6879039252919));
#5658=CARTESIAN_POINT('Ctrl Pts',(-26.1364187282489,1.32853748653122,-2.6897982252467));
#5659=CARTESIAN_POINT('Ctrl Pts',(-26.1932111473027,1.31546058553579,-2.69623084419525));
#5660=CARTESIAN_POINT('Ctrl Pts',(-26.2306587701737,1.30460495425469,-2.70152087608486));
#5661=CARTESIAN_POINT('Ctrl Pts',(-26.2769393229609,1.2883550701772,-2.70927245589677));
#5662=CARTESIAN_POINT('Ctrl Pts',(-26.2861735714613,1.28496732277494,-2.7108812019877));
#5663=CARTESIAN_POINT('Ctrl Pts',(-26.3045800008344,1.27792560939945,-2.71420782302654));
#5664=CARTESIAN_POINT('Ctrl Pts',(-26.3137695365298,1.27426364167248,-2.71592937831152));
#5665=CARTESIAN_POINT('Ctrl Pts',(-26.3411342135086,1.26291934373526,-2.72123265364053));
#5666=CARTESIAN_POINT('Ctrl Pts',(-26.359108489593,1.25488165967843,-2.72495179584751));
#5667=CARTESIAN_POINT('Ctrl Pts',(-26.3945729485002,1.23786371810423,-2.73272458713573));
#5668=CARTESIAN_POINT('Ctrl Pts',(-26.4120572689161,1.2288861049134,-2.73677701321045));
#5669=CARTESIAN_POINT('Ctrl Pts',(-26.4465442238038,1.21000802381103,-2.74517577574545));
#5670=CARTESIAN_POINT('Ctrl Pts',(-26.4635468416443,1.20010753017732,-2.74952213668882));
#5671=CARTESIAN_POINT('Ctrl Pts',(-26.4970804298005,1.17938992628659,-2.75847230162352));
#5672=CARTESIAN_POINT('Ctrl Pts',(-26.5136113919084,1.16857280798543,-2.76307612855274));
#5673=CARTESIAN_POINT('Ctrl Pts',(-26.5462078840406,1.14602038731631,-2.77250596727388));
#5674=CARTESIAN_POINT('Ctrl Pts',(-26.562273493867,1.1342850254395,-2.77733202823839));
#5675=CARTESIAN_POINT('Ctrl Pts',(-26.5939414283119,1.10988700911992,-2.78717177677759));
#5676=CARTESIAN_POINT('Ctrl Pts',(-26.6095473445415,1.09722131473956,-2.79218666030943));
#5677=CARTESIAN_POINT('Ctrl Pts',(-26.6402811143626,1.0709566148845,-2.8023656091679));
#5678=CARTESIAN_POINT('Ctrl Pts',(-26.6552948463125,1.05745575069761,-2.80749156457345));
#5679=CARTESIAN_POINT('Ctrl Pts',(-26.6846546110444,1.02971343125002,-2.817784903976));
#5680=CARTESIAN_POINT('Ctrl Pts',(-26.6989977054847,1.0154744409772,-2.82295134426973));
#5681=CARTESIAN_POINT('Ctrl Pts',(-26.7270250638549,0.986265666309434,-2.83328830718171));
#5682=CARTESIAN_POINT('Ctrl Pts',(-26.7407092830319,0.971295850373597,-2.83845888576662));
#5683=CARTESIAN_POINT('Ctrl Pts',(-26.7807869864753,0.925288343298038,-2.85392552592912));
#5684=CARTESIAN_POINT('Ctrl Pts',(-26.8062104528913,0.893151438987838,-2.86417785822885));
#5685=CARTESIAN_POINT('Ctrl Pts',(-26.8423944800688,0.842704105273585,-2.87926390500452));
#5686=CARTESIAN_POINT('Ctrl Pts',(-26.854135591242,0.825504489114966,-2.88424645343755));
#5687=CARTESIAN_POINT('Ctrl Pts',(-26.8712462612575,0.799138658144538,-2.89161951102431));
#5688=CARTESIAN_POINT('Ctrl Pts',(-26.876870779104,0.790247883055742,-2.89406240563576));
#5689=CARTESIAN_POINT('Ctrl Pts',(-26.8879469072247,0.772281655830631,-2.89890846334945));
#5690=CARTESIAN_POINT('Ctrl Pts',(-26.893409269784,0.763187520111317,-2.90131641792487));
#5691=CARTESIAN_POINT('Ctrl Pts',(-26.9094749238114,0.735724555729973,-2.90844791977076));
#5692=CARTESIAN_POINT('Ctrl Pts',(-26.9197549867311,0.717184843056236,-2.91307769758814));
#5693=CARTESIAN_POINT('Ctrl Pts',(-26.9394913365264,0.679605859000127,-2.92207317082987));
#5694=CARTESIAN_POINT('Ctrl Pts',(-26.9489438557812,0.66057330364731,-2.92643722327291));
#5695=CARTESIAN_POINT('Ctrl Pts',(-26.9760661551845,0.602745633656238,-2.93909124911831));
#5696=CARTESIAN_POINT('Ctrl Pts',(-26.9925036507446,0.563222175536771,-2.94694362837257));
#5697=CARTESIAN_POINT('Ctrl Pts',(-27.0220715762404,0.482184664459273,-2.96128235245645));
#5698=CARTESIAN_POINT('Ctrl Pts',(-27.0352035249924,0.440658030285019,-2.96777002657));
#5699=CARTESIAN_POINT('Ctrl Pts',(-27.0523216883035,0.376833839229868,-2.97631699067074));
#5700=CARTESIAN_POINT('Ctrl Pts',(-27.0576005303158,0.355274412887374,-2.97897027612798));
#5701=CARTESIAN_POINT('Ctrl Pts',(-27.0672600591522,0.311662753136127,-2.98384821443584));
#5702=CARTESIAN_POINT('Ctrl Pts',(-27.0716114828177,0.289741794867057,-2.9860580250039));
#5703=CARTESIAN_POINT('Ctrl Pts',(-27.0793660357628,0.245626078050727,-2.99001014183973));
#5704=CARTESIAN_POINT('Ctrl Pts',(-27.0827661298392,0.223449095191074,-2.99175090619715));
#5705=CARTESIAN_POINT('Ctrl Pts',(-27.088612570746,0.178789136156299,-2.99475173451271));
#5706=CARTESIAN_POINT('Ctrl Pts',(-27.0910448696872,0.156404671590301,-2.99600458388059));
#5707=CARTESIAN_POINT('Ctrl Pts',(-27.096853679446,0.0893800225646476,-2.9990010619891));
#5708=CARTESIAN_POINT('Ctrl Pts',(-27.098776248484,0.0447217666279721,-2.99999873125252));
#5709=CARTESIAN_POINT('Ctrl Pts',(-27.0987810099015,-0.0221932423036774,
-3.00000122002206));
#5710=CARTESIAN_POINT('Ctrl Pts',(-27.0983026039981,-0.0444881794306497,
-2.99975332625577));
#5711=CARTESIAN_POINT('Ctrl Pts',(-27.0963847740834,-0.0890579105479476,
-2.99876106205554));
#5712=CARTESIAN_POINT('Ctrl Pts',(-27.0949453773136,-0.111332705013248,
-2.99801669216856));
#5713=CARTESIAN_POINT('Ctrl Pts',(-27.0910975380372,-0.155862012281646,
-2.99603172453301));
#5714=CARTESIAN_POINT('Ctrl Pts',(-27.0886879051299,-0.178121225730192,
-2.99479051237394));
#5715=CARTESIAN_POINT('Ctrl Pts',(-27.0828889596371,-0.222600296296536,
-2.99181384430895));
#5716=CARTESIAN_POINT('Ctrl Pts',(-27.0794840506901,-0.24488839674227,-2.99007048023225));
#5717=CARTESIAN_POINT('Ctrl Pts',(-27.071775952777,-0.288869899263924,-2.98614166251469));
#5718=CARTESIAN_POINT('Ctrl Pts',(-27.0674608269688,-0.310670331278561,
-2.98395006519913));
#5719=CARTESIAN_POINT('Ctrl Pts',(-27.0579363802439,-0.353839366034688,
-2.9791394357373));
#5720=CARTESIAN_POINT('Ctrl Pts',(-27.0527258255725,-0.375218389994937,
-2.97651976178012));
#5721=CARTESIAN_POINT('Ctrl Pts',(-27.0357695640527,-0.438751704381787,
-2.96805078583667));
#5722=CARTESIAN_POINT('Ctrl Pts',(-27.0226990393997,-0.480310373169669,
-2.96158999423888));
#5723=CARTESIAN_POINT('Ctrl Pts',(-27.0004754778274,-0.541446390227559,
-2.95080792183841));
#5724=CARTESIAN_POINT('Ctrl Pts',(-26.9926233391618,-0.561639756422953,
-2.94702858491464));
#5725=CARTESIAN_POINT('Ctrl Pts',(-26.9801906409175,-0.591614002592807,
-2.94110512698185));
#5726=CARTESIAN_POINT('Ctrl Pts',(-26.9759329233523,-0.601561926835125,
-2.9390861971729));
#5727=CARTESIAN_POINT('Ctrl Pts',(-26.9671986892834,-0.621350277064196,
-2.93496653895837));
#5728=CARTESIAN_POINT('Ctrl Pts',(-26.9627160190822,-0.63120305480576,-2.932862972483));
#5729=CARTESIAN_POINT('Ctrl Pts',(-26.949000010224,-0.660466243653679,-2.92646286445819));
#5730=CARTESIAN_POINT('Ctrl Pts',(-26.9394863006083,-0.679616625492289,
-2.92207081256717));
#5731=CARTESIAN_POINT('Ctrl Pts',(-26.9197260539462,-0.717238752620477,
-2.91306457362862));
#5732=CARTESIAN_POINT('Ctrl Pts',(-26.9094809907086,-0.735707812001506,
-2.90845102679016));
#5733=CARTESIAN_POINT('Ctrl Pts',(-26.8776648850953,-0.790113953263625,
-2.8943267049494));
#5734=CARTESIAN_POINT('Ctrl Pts',(-26.8550156533739,-0.825052204529002,
-2.88453180649776));
#5735=CARTESIAN_POINT('Ctrl Pts',(-26.8188825262082,-0.875510966128818,
-2.86945837323707));
#5736=CARTESIAN_POINT('Ctrl Pts',(-26.8064775830923,-0.892005171014228,
-2.86437028648305));
#5737=CARTESIAN_POINT('Ctrl Pts',(-26.7809368156929,-0.924343274785419,
-2.85409879125165));
#5738=CARTESIAN_POINT('Ctrl Pts',(-26.767806005017,-0.940181255880803,-2.84891729113089));
#5739=CARTESIAN_POINT('Ctrl Pts',(-26.7475346890206,-0.963464821076124,
-2.84109226874023));
#5740=CARTESIAN_POINT('Ctrl Pts',(-26.7406844898386,-0.971142790692552,
-2.83847640424402));
#5741=CARTESIAN_POINT('Ctrl Pts',(-26.7268665710498,-0.986257223502061,
-2.83326015443131));
#5742=CARTESIAN_POINT('Ctrl Pts',(-26.7198861854429,-0.993708406579362,
-2.83065485672359));
#5743=CARTESIAN_POINT('Ctrl Pts',(-26.6987543184742,-1.01572209996893,-2.82286262012559));
#5744=CARTESIAN_POINT('Ctrl Pts',(-26.6843926989096,-1.02996746343674,-2.81769174714818));
#5745=CARTESIAN_POINT('Ctrl Pts',(-26.6405194665222,-1.07140391340387,-2.80231410558904));
#5746=CARTESIAN_POINT('Ctrl Pts',(-26.6101987968579,-1.09732460419766,-2.79223276559477));
#5747=CARTESIAN_POINT('Ctrl Pts',(-26.5630918828768,-1.13367250400703,-2.77758169296716));
#5748=CARTESIAN_POINT('Ctrl Pts',(-26.5471174957754,-1.14536614557727,-2.77277626806029));
#5749=CARTESIAN_POINT('Ctrl Pts',(-26.514612671107,-1.167903545887,-2.76335903848249));
#5750=CARTESIAN_POINT('Ctrl Pts',(-26.4980822787532,-1.17874735889938,-2.7587471803173));
#5751=CARTESIAN_POINT('Ctrl Pts',(-26.46444880388,-1.19957259205025,-2.74975580028194));
#5752=CARTESIAN_POINT('Ctrl Pts',(-26.4473524929256,-1.20955009125369,-2.74537799392286));
#5753=CARTESIAN_POINT('Ctrl Pts',(-26.4212416835811,-1.22386590602099,-2.73901119026752));
#5754=CARTESIAN_POINT('Ctrl Pts',(-26.4124619953677,-1.22852739949809,-2.73692306012723));
#5755=CARTESIAN_POINT('Ctrl Pts',(-26.3948577516024,-1.23757286419293,-2.73284480288515));
#5756=CARTESIAN_POINT('Ctrl Pts',(-26.3860147393496,-1.24196779569831,-2.73084989444485));
#5757=CARTESIAN_POINT('Ctrl Pts',(-26.3416451282571,-1.26327195668704,-2.72112034953696));
#5758=CARTESIAN_POINT('Ctrl Pts',(-26.3055754632133,-1.27824521948247,-2.71409222828942));
#5759=CARTESIAN_POINT('Ctrl Pts',(-26.2323060083433,-1.30407984829822,-2.70177412725945));
#5760=CARTESIAN_POINT('Ctrl Pts',(-26.1951016228417,-1.31494638090081,-2.69648191406169));
#5761=CARTESIAN_POINT('Ctrl Pts',(-26.1384100565222,-1.32811542764141,-2.69000670173171));
#5762=CARTESIAN_POINT('Ctrl Pts',(-26.1193651709025,-1.33198245867611,-2.68809214937698));
#5763=CARTESIAN_POINT('Ctrl Pts',(-26.0809718351375,-1.33864905018688,-2.68477846139787));
#5764=CARTESIAN_POINT('Ctrl Pts',(-26.0616267046488,-1.34144791557871,-2.68337970984734));
#5765=CARTESIAN_POINT('Ctrl Pts',(-26.0323637266099,-1.34482464575182,-2.68168810040417));
#5766=CARTESIAN_POINT('Ctrl Pts',(-26.0225572452852,-1.34581322849438,-2.68119198692628));
#5767=CARTESIAN_POINT('Ctrl Pts',(-26.0029866629929,-1.34750144912675,-2.68034392500146));
#5768=CARTESIAN_POINT('Ctrl Pts',(-25.993207230682,-1.34820337332278,-2.67999083517031));
#5769=CARTESIAN_POINT('Ctrl Pts',(-25.9639248638171,-1.34988238530038,-2.67914574940456));
#5770=CARTESIAN_POINT('Ctrl Pts',(-25.944430250381,-1.35043878696277,-2.67886501715932));
#5771=CARTESIAN_POINT('Ctrl Pts',(-25.8861245564454,-1.35043705000303,-2.67886596390227));
#5772=CARTESIAN_POINT('Ctrl Pts',(-25.8474104061639,-1.34822092631382,-2.67998650091243));
#5773=CARTESIAN_POINT('Ctrl Pts',(-25.7896109432291,-1.34160967645964,-2.68329876772692));
#5774=CARTESIAN_POINT('Ctrl Pts',(-25.7703875060739,-1.33885738792583,-2.68467452923362));
#5775=CARTESIAN_POINT('Ctrl Pts',(-25.7320267909422,-1.33224993750147,-2.68795954661435));
#5776=CARTESIAN_POINT('Ctrl Pts',(-25.7128830927771,-1.32839290578458,-2.68986973704836));
#5777=CARTESIAN_POINT('Ctrl Pts',(-25.684251825295,-1.32177548884069,-2.69312428914528));
#5778=CARTESIAN_POINT('Ctrl Pts',(-25.6747142093514,-1.31942848978328,-2.69427521202406));
#5779=CARTESIAN_POINT('Ctrl Pts',(-25.6556603366635,-1.31445289803523,-2.69670614956339));
#5780=CARTESIAN_POINT('Ctrl Pts',(-25.6461500334678,-1.31182518416257,-2.69798570492286));
#5781=CARTESIAN_POINT('Ctrl Pts',(-25.6178200674555,-1.30356617188209,-2.70199101363684));
#5782=CARTESIAN_POINT('Ctrl Pts',(-25.5991463885073,-1.29754777172781,-2.70488904077813));
#5783=CARTESIAN_POINT('Ctrl Pts',(-25.5622143033361,-1.28450992377735,-2.711104791713));
#5784=CARTESIAN_POINT('Ctrl Pts',(-25.5439552645306,-1.27749068571576,-2.71442241845669));
#5785=CARTESIAN_POINT('Ctrl Pts',(-25.5078400226815,-1.26246775944475,-2.72144201858098));
#5786=CARTESIAN_POINT('Ctrl Pts',(-25.4899838433394,-1.25446401700334,-2.72514402265192));
#5787=CARTESIAN_POINT('Ctrl Pts',(-25.4370074508209,-1.22898778436132,-2.736775538613));
#5788=CARTESIAN_POINT('Ctrl Pts',(-25.402476169391,-1.21005033530757,-2.74523167785092));
#5789=CARTESIAN_POINT('Ctrl Pts',(-25.3602840547609,-1.18392811236617,-2.7565104471187));
#5790=CARTESIAN_POINT('Ctrl Pts',(-25.3518921545878,-1.17857779567388,-2.75880270804698));
#5791=CARTESIAN_POINT('Ctrl Pts',(-25.33521027166,-1.16763346103173,-2.76345258994632));
#5792=CARTESIAN_POINT('Ctrl Pts',(-25.3269101970962,-1.16203150593469,-2.76581339519711));
#5793=CARTESIAN_POINT('Ctrl Pts',(-25.3022697723606,-1.14492960216067,-2.77295715687364));
#5794=CARTESIAN_POINT('Ctrl Pts',(-25.2861659342133,-1.13312196993095,-2.77780680847141));
#5795=CARTESIAN_POINT('Ctrl Pts',(-25.2545677370148,-1.10869517847092,-2.78764614588441));
#5796=CARTESIAN_POINT('Ctrl Pts',(-25.2390760976615,-1.09607817216592,-2.79263498420857));
#5797=CARTESIAN_POINT('Ctrl Pts',(-25.2086929585038,-1.0700438882078,-2.80271360615569));
#5798=CARTESIAN_POINT('Ctrl Pts',(-25.1938014786094,-1.05662659440153,-2.80780342156984));
#5799=CARTESIAN_POINT('Ctrl Pts',(-25.1646092945331,-1.02899172455792,-2.81804822663801));
#5800=CARTESIAN_POINT('Ctrl Pts',(-25.1503085987059,-1.01477414783797,-2.82320324630944));
#5801=CARTESIAN_POINT('Ctrl Pts',(-25.122293720064,-0.98553195302638,-2.83354369456912));
#5802=CARTESIAN_POINT('Ctrl Pts',(-25.1085795345898,-0.970507349552267,
-2.83872915299998));
#5803=CARTESIAN_POINT('Ctrl Pts',(-25.0817384653232,-0.9396374697407,-2.84909618968299));
#5804=CARTESIAN_POINT('Ctrl Pts',(-25.0686121956922,-0.923792524689856,
-2.85427759753642));
#5805=CARTESIAN_POINT('Ctrl Pts',(-25.0493658734545,-0.89939302142587,-2.86202163910769));
#5806=CARTESIAN_POINT('Ctrl Pts',(-25.043017487774,-0.89114441813432,-2.86460120904707));
#5807=CARTESIAN_POINT('Ctrl Pts',(-25.0305207080603,-0.874501431709215,
-2.86972568743742));
#5808=CARTESIAN_POINT('Ctrl Pts',(-25.0243713909441,-0.866107457626747,
-2.87227076450331));
#5809=CARTESIAN_POINT('Ctrl Pts',(-24.9941176023294,-0.823767677123209,
-2.88490127988302));
#5810=CARTESIAN_POINT('Ctrl Pts',(-24.97147225811,-0.788728779396106,-2.89470358965755));
#5811=CARTESIAN_POINT('Ctrl Pts',(-24.9292312229828,-0.716311799075431,
-2.9134684860099));
#5812=CARTESIAN_POINT('Ctrl Pts',(-24.9096337112948,-0.678934474646847,
-2.92243229488294));
#5813=CARTESIAN_POINT('Ctrl Pts',(-24.8825415051001,-0.621060303181762,
-2.93507687968496));
#5814=CARTESIAN_POINT('Ctrl Pts',(-24.8738954614447,-0.601467085362859,
-2.93915828390893));
#5815=CARTESIAN_POINT('Ctrl Pts',(-24.8573860335644,-0.561660534816688,
-2.94702417229759));
#5816=CARTESIAN_POINT('Ctrl Pts',(-24.8495222347111,-0.541445118061438,
-2.95080889756673));
#5817=CARTESIAN_POINT('Ctrl Pts',(-24.8383296294352,-0.510647204231348,
-2.95623934885627));
#5818=CARTESIAN_POINT('Ctrl Pts',(-24.8346943538624,-0.500285572119669,
-2.95801084324021));
#5819=CARTESIAN_POINT('Ctrl Pts',(-24.8276507980447,-0.479467813925564,
-2.96145644444383));
#5820=CARTESIAN_POINT('Ctrl Pts',(-24.8242486897808,-0.469031540585879,
-2.96312749437883));
#5821=CARTESIAN_POINT('Ctrl Pts',(-24.8143975220266,-0.437635545407871,
-2.967983313185));
#5822=CARTESIAN_POINT('Ctrl Pts',(-24.8082918810615,-0.416559413593511,
-2.97101630939715));
#5823=CARTESIAN_POINT('Ctrl Pts',(-24.79700967936,-0.374165575587155,-2.97665244169902));
#5824=CARTESIAN_POINT('Ctrl Pts',(-24.7918302021315,-0.352839925216633,
-2.97925701409689));
#5825=CARTESIAN_POINT('Ctrl Pts',(-24.782389529693,-0.309931149531079,-2.98402597733368));
#5826=CARTESIAN_POINT('Ctrl Pts',(-24.77812834015,-0.288348024079469,-2.98619038155605));
#5827=CARTESIAN_POINT('Ctrl Pts',(-24.7705262413241,-0.24492258799079,-2.99006529803462));
#5828=CARTESIAN_POINT('Ctrl Pts',(-24.767185323199,-0.223080280695769,-2.9917758240911));
#5829=CARTESIAN_POINT('Ctrl Pts',(-24.7614327168412,-0.179133051352737,
-2.99472848957151));
#5830=CARTESIAN_POINT('Ctrl Pts',(-24.7590210045444,-0.157028136357559,
-2.99597064391189));
#5831=CARTESIAN_POINT('Ctrl Pts',(-24.7551430015195,-0.112550450866729,
-2.99797103284412));
#5832=CARTESIAN_POINT('Ctrl Pts',(-24.7536770371529,-0.0901765544388105,
-2.99872909299961));
#5833=CARTESIAN_POINT('Ctrl Pts',(-24.7522040612047,-0.0564128194848313,
-2.9994911778993));
#5834=CARTESIAN_POINT('Ctrl Pts',(-24.7518343852008,-0.0451068922413159,
-2.999682558101));
#5835=CARTESIAN_POINT('Ctrl Pts',(-24.7513427166217,-0.0225174680468727,
-2.99993712712975));
#5836=CARTESIAN_POINT('Ctrl Pts',(-24.7512203639079,-0.0112452244724441,
-3.00000050164314));
#5837=CARTESIAN_POINT('Ctrl Pts',(-24.7512205732181,1.27647900817359E-15,
-3.00000039251396));
#5838=CARTESIAN_POINT('Ctrl Pts',(-24.925,9.1987778071817E-16,-2.60755260924174));
#5839=CARTESIAN_POINT('Ctrl Pts',(-24.9250003566431,0.0166541858892919,
-2.60755241953505));
#5840=CARTESIAN_POINT('Ctrl Pts',(-24.9254160783661,0.0332581559508148,
-2.60733265858178));
#5841=CARTESIAN_POINT('Ctrl Pts',(-24.9270649354643,0.0663304974791159,
-2.60646231020682));
#5842=CARTESIAN_POINT('Ctrl Pts',(-24.9282977615931,0.0828051219601012,
-2.60581189691126));
#5843=CARTESIAN_POINT('Ctrl Pts',(-24.9332076090917,0.132046707858214,-2.60322787601198));
#5844=CARTESIAN_POINT('Ctrl Pts',(-24.9380956117425,0.164639289236405,-2.60066047948669));
#5845=CARTESIAN_POINT('Ctrl Pts',(-24.9478395671871,0.213143553563254,-2.59559297392187));
#5846=CARTESIAN_POINT('Ctrl Pts',(-24.9514952030343,0.229263645988802,-2.59369843168222));
#5847=CARTESIAN_POINT('Ctrl Pts',(-24.9575851418319,0.253332291674964,-2.59055979222182));
#5848=CARTESIAN_POINT('Ctrl Pts',(-24.9597188141185,0.261344691370318,-2.58946279377858));
#5849=CARTESIAN_POINT('Ctrl Pts',(-24.9641906612921,0.2773345184445,-2.5871703966394));
#5850=CARTESIAN_POINT('Ctrl Pts',(-24.966530765891,0.28531677926617,-2.58597403111896));
#5851=CARTESIAN_POINT('Ctrl Pts',(-24.973820513222,0.309081961524918,-2.58225915775742));
#5852=CARTESIAN_POINT('Ctrl Pts',(-24.9790484377681,0.32472379379895,-2.57961022574372));
#5853=CARTESIAN_POINT('Ctrl Pts',(-24.9902256908821,0.355621851323136,-2.57399040352468));
#5854=CARTESIAN_POINT('Ctrl Pts',(-24.9961745187184,0.370877172015151,-2.57101975041035));
#5855=CARTESIAN_POINT('Ctrl Pts',(-25.0150836576248,0.416076046241271,-2.56166046299739));
#5856=CARTESIAN_POINT('Ctrl Pts',(-25.0291043543913,0.445453982261496,-2.55482429402179));
#5857=CARTESIAN_POINT('Ctrl Pts',(-25.0522383184702,0.488417442273934,-2.54380826092922));
#5858=CARTESIAN_POINT('Ctrl Pts',(-25.0603014453932,0.502555351656385,-2.54000886254706));
#5859=CARTESIAN_POINT('Ctrl Pts',(-25.0771344181921,0.530461627229326,-2.53217843551043));
#5860=CARTESIAN_POINT('Ctrl Pts',(-25.0859109306211,0.544239963564886,-2.52814434334756));
#5861=CARTESIAN_POINT('Ctrl Pts',(-25.1041597996001,0.571392063284264,-2.51987677295434));
#5862=CARTESIAN_POINT('Ctrl Pts',(-25.1135652356457,0.584667955785163,-2.51567359591457));
#5863=CARTESIAN_POINT('Ctrl Pts',(-25.1329503931644,0.610672109363501,-2.50714732573441));
#5864=CARTESIAN_POINT('Ctrl Pts',(-25.1429262744659,0.623394578020974,-2.50282595067222));
#5865=CARTESIAN_POINT('Ctrl Pts',(-25.1736949347874,0.660743188336082,-2.48973044146156));
#5866=CARTESIAN_POINT('Ctrl Pts',(-25.1953265696652,0.684552408790024,-2.4808244164163));
#5867=CARTESIAN_POINT('Ctrl Pts',(-25.2294621790932,0.718669526189459,-2.46737442476457));
#5868=CARTESIAN_POINT('Ctrl Pts',(-25.2411226141971,0.729775262858413,-2.46287588038061));
#5869=CARTESIAN_POINT('Ctrl Pts',(-25.2650163395358,0.751453108570395,-2.45387816269177));
#5870=CARTESIAN_POINT('Ctrl Pts',(-25.2772554632753,0.762029504500182,-2.44937698167526));
#5871=CARTESIAN_POINT('Ctrl Pts',(-25.3022971286317,0.782626892006878,-2.44041267983555));
#5872=CARTESIAN_POINT('Ctrl Pts',(-25.315157197433,0.792689421921388,-2.43593042229926));
#5873=CARTESIAN_POINT('Ctrl Pts',(-25.3412327555041,0.812083164942921,-2.4271128386545));
#5874=CARTESIAN_POINT('Ctrl Pts',(-25.3544672859955,0.821434074532995,-2.4227697238751));
#5875=CARTESIAN_POINT('Ctrl Pts',(-25.3813264071519,0.839452527788184,-2.41424554238548));
#5876=CARTESIAN_POINT('Ctrl Pts',(-25.3949513697869,0.848120793930839,-2.41006421940508));
#5877=CARTESIAN_POINT('Ctrl Pts',(-25.4225940554056,0.864782458141239,-2.40189271204071));
#5878=CARTESIAN_POINT('Ctrl Pts',(-25.4366117834694,0.872775835903154,-2.39790249830953));
#5879=CARTESIAN_POINT('Ctrl Pts',(-25.479261734589,0.89574572391242,-2.38626398652599));
#5880=CARTESIAN_POINT('Ctrl Pts',(-25.5084958123966,0.909716954879009,-2.37894574292179));
#5881=CARTESIAN_POINT('Ctrl Pts',(-25.5535776615725,0.928607298291761,-2.36882679203485));
#5882=CARTESIAN_POINT('Ctrl Pts',(-25.5688253899689,0.934563660377401,-2.36559439343672));
#5883=CARTESIAN_POINT('Ctrl Pts',(-25.5920023693806,0.942963605388764,-2.36098892152974));
#5884=CARTESIAN_POINT('Ctrl Pts',(-25.5997879839068,0.945677166439889,-2.35949277008248));
#5885=CARTESIAN_POINT('Ctrl Pts',(-25.6154612044866,0.950922793268217,-2.35658631440841));
#5886=CARTESIAN_POINT('Ctrl Pts',(-25.6233613960042,0.953458374961467,-2.35517402568801));
#5887=CARTESIAN_POINT('Ctrl Pts',(-25.6470876486476,0.960748669979317,-2.35109499689055));
#5888=CARTESIAN_POINT('Ctrl Pts',(-25.6629694924038,0.965199959788433,-2.34857921219018));
#5889=CARTESIAN_POINT('Ctrl Pts',(-25.6948784413748,0.97330109610864,-2.34396841563554));
#5890=CARTESIAN_POINT('Ctrl Pts',(-25.710902645268,0.976950283068507,-2.34187376666203));
#5891=CARTESIAN_POINT('Ctrl Pts',(-25.7591844222773,0.986703415822537,-2.33624500537069));
#5892=CARTESIAN_POINT('Ctrl Pts',(-25.791650783833,0.991615665333942,-2.33336629059961));
#5893=CARTESIAN_POINT('Ctrl Pts',(-25.8407756179032,0.996582697577232,-2.33044584989519));
#5894=CARTESIAN_POINT('Ctrl Pts',(-25.8572215351598,0.997837487879419,-2.32970524177098));
#5895=CARTESIAN_POINT('Ctrl Pts',(-25.8902578614934,0.999533165226665,-2.3287035410661));
#5896=CARTESIAN_POINT('Ctrl Pts',(-25.9068578724972,0.999973524878361,-2.32844279123644));
#5897=CARTESIAN_POINT('Ctrl Pts',(-25.940167362761,1.0000242628141,-2.32841276730313));
#5898=CARTESIAN_POINT('Ctrl Pts',(-25.9569704588412,0.999628762374181,-2.32864698234143));
#5899=CARTESIAN_POINT('Ctrl Pts',(-25.9903233075244,0.998003316619995,-2.32960735397221));
#5900=CARTESIAN_POINT('Ctrl Pts',(-26.0069064582144,0.99677776727011,-2.33033089082928));
#5901=CARTESIAN_POINT('Ctrl Pts',(-26.0398870987565,0.993516757651968,-2.33224874868743));
#5902=CARTESIAN_POINT('Ctrl Pts',(-26.0562852280577,0.991481744891028,-2.3334427918359));
#5903=CARTESIAN_POINT('Ctrl Pts',(-26.0889006503167,0.986614637292694,-2.3362833255874));
#5904=CARTESIAN_POINT('Ctrl Pts',(-26.1051179364934,0.983782507538744,-2.33792982096872));
#5905=CARTESIAN_POINT('Ctrl Pts',(-26.1535021710044,0.974099057442963,-2.3435209510113));
#5906=CARTESIAN_POINT('Ctrl Pts',(-26.1854056292135,0.966060458399383,-2.34811896256439));
#5907=CARTESIAN_POINT('Ctrl Pts',(-26.2248342916283,0.954027413144458,-2.35485651240158));
#5908=CARTESIAN_POINT('Ctrl Pts',(-26.2327013987641,0.951518784920254,-2.35625480890823));
#5909=CARTESIAN_POINT('Ctrl Pts',(-26.2483827345867,0.946304393522069,-2.35914625498641));
#5910=CARTESIAN_POINT('Ctrl Pts',(-26.2562117486977,0.943592705045449,-2.36064260344911));
#5911=CARTESIAN_POINT('Ctrl Pts',(-26.2795250530157,0.935192248164097,-2.36525212598659));
#5912=CARTESIAN_POINT('Ctrl Pts',(-26.2948382163531,0.929240340102425,-2.36848474521894));
#5913=CARTESIAN_POINT('Ctrl Pts',(-26.325052120344,0.916638547977858,-2.37524073173656));
#5914=CARTESIAN_POINT('Ctrl Pts',(-26.3399478665267,0.909990622039622,-2.37876303600402));
#5915=CARTESIAN_POINT('Ctrl Pts',(-26.3693289871196,0.89601139589608,-2.38606310676973));
#5916=CARTESIAN_POINT('Ctrl Pts',(-26.3838143473607,0.888680076643437,-2.38984089454832));
#5917=CARTESIAN_POINT('Ctrl Pts',(-26.4123832482896,0.873338683184519,-2.39762023550669));
#5918=CARTESIAN_POINT('Ctrl Pts',(-26.4264667819849,0.865328603021504,-2.40162180862373));
#5919=CARTESIAN_POINT('Ctrl Pts',(-26.4542373250601,0.848628527049356,-2.40981807440536));
#5920=CARTESIAN_POINT('Ctrl Pts',(-26.4679244024272,0.839938487173804,-2.41401280980997));
#5921=CARTESIAN_POINT('Ctrl Pts',(-26.4949038618745,0.821871746929689,-2.42256536268357));
#5922=CARTESIAN_POINT('Ctrl Pts',(-26.5081993038235,0.812492795486006,-2.4269242196594));
#5923=CARTESIAN_POINT('Ctrl Pts',(-26.5343829028199,0.793043775382973,-2.43577160005358));
#5924=CARTESIAN_POINT('Ctrl Pts',(-26.5471738340693,0.783046380384102,-2.44022699893485));
#5925=CARTESIAN_POINT('Ctrl Pts',(-26.5721868510483,0.762503182417989,-2.44917380576989));
#5926=CARTESIAN_POINT('Ctrl Pts',(-26.5844064334615,0.751959204775379,-2.45366439347183));
#5927=CARTESIAN_POINT('Ctrl Pts',(-26.6082843084103,0.730330096168269,-2.46264911716721));
#5928=CARTESIAN_POINT('Ctrl Pts',(-26.6199425628188,0.719244941847823,-2.46714330180597));
#5929=CARTESIAN_POINT('Ctrl Pts',(-26.6540867150583,0.685176365586002,-2.4805866593511));
#5930=CARTESIAN_POINT('Ctrl Pts',(-26.6757462073237,0.661378975879614,-2.48949782346476));
#5931=CARTESIAN_POINT('Ctrl Pts',(-26.706573146655,0.624022706324936,-2.50261037529356));
#5932=CARTESIAN_POINT('Ctrl Pts',(-26.7165759724886,0.611286384102533,-2.50694112711596));
#5933=CARTESIAN_POINT('Ctrl Pts',(-26.7311533876529,0.591762476370502,-2.51334967146032));
#5934=CARTESIAN_POINT('Ctrl Pts',(-26.7359451890069,0.585178854079478,-2.51547299658856));
#5935=CARTESIAN_POINT('Ctrl Pts',(-26.7453814833122,0.571874856074331,-2.51968511284942));
#5936=CARTESIAN_POINT('Ctrl Pts',(-26.7500351366602,0.565140645160058,-2.52177806865427));
#5937=CARTESIAN_POINT('Ctrl Pts',(-26.7637222516845,0.544804309725441,-2.52797665659195));
#5938=CARTESIAN_POINT('Ctrl Pts',(-26.7724803391795,0.531075645530331,-2.53200078580807));
#5939=CARTESIAN_POINT('Ctrl Pts',(-26.7892946991393,0.503248393728805,-2.53981950802604));
#5940=CARTESIAN_POINT('Ctrl Pts',(-26.7973477617837,0.489154779345304,-2.54361267297452));
#5941=CARTESIAN_POINT('Ctrl Pts',(-26.8204545728126,0.446333368005566,-2.55461135090606));
#5942=CARTESIAN_POINT('Ctrl Pts',(-26.834458477791,0.417066232433272,-2.56143651401678));
#5943=CARTESIAN_POINT('Ctrl Pts',(-26.8596488370896,0.357057925052848,-2.57389950485306));
#5944=CARTESIAN_POINT('Ctrl Pts',(-26.8708365853539,0.326307436876508,-2.57953848796631));
#5945=CARTESIAN_POINT('Ctrl Pts',(-26.8854203844307,0.279045599412755,-2.58696737317912));
#5946=CARTESIAN_POINT('Ctrl Pts',(-26.8899176876621,0.263080836121059,-2.5892735666817));
#5947=CARTESIAN_POINT('Ctrl Pts',(-26.8981471118759,0.230786385702432,-2.59351339304776));
#5948=CARTESIAN_POINT('Ctrl Pts',(-26.901854302142,0.21455390787461,-2.59543412523401));
#5949=CARTESIAN_POINT('Ctrl Pts',(-26.9084607843892,0.18188620301005,-2.59886924230701));
#5950=CARTESIAN_POINT('Ctrl Pts',(-26.9113574905324,0.165464138876775,-2.60038228698979));
#5951=CARTESIAN_POINT('Ctrl Pts',(-26.9163383589761,0.132393422445161,-2.60299055921657));
#5952=CARTESIAN_POINT('Ctrl Pts',(-26.9184105531932,0.115817718038398,-2.60407951595308));
#5953=CARTESIAN_POINT('Ctrl Pts',(-26.9233593618272,0.0661859402484169,
-2.60668400705037));
#5954=CARTESIAN_POINT('Ctrl Pts',(-26.9249972922528,0.0331164849794912,
-2.60755116529973));
#5955=CARTESIAN_POINT('Ctrl Pts',(-26.9250013487368,-0.0164341042586774,
-2.60755332849862));
#5956=CARTESIAN_POINT('Ctrl Pts',(-26.924593771391,-0.0329435135702297,
-2.60733786318111));
#5957=CARTESIAN_POINT('Ctrl Pts',(-26.9229598784543,-0.0659474161951027,
-2.60647540292583));
#5958=CARTESIAN_POINT('Ctrl Pts',(-26.9217335860717,-0.0824419098590701,
-2.60582840846347));
#5959=CARTESIAN_POINT('Ctrl Pts',(-26.9184554239328,-0.115415878608659,
-2.60410310617676));
#5960=CARTESIAN_POINT('Ctrl Pts',(-26.9164025400161,-0.13189883452203,-2.60302426431672));
#5961=CARTESIAN_POINT('Ctrl Pts',(-26.9114621352338,-0.164835602978563,
-2.60043699179504));
#5962=CARTESIAN_POINT('Ctrl Pts',(-26.9085613270678,-0.181339949722123,
-2.59892168747798));
#5963=CARTESIAN_POINT('Ctrl Pts',(-26.9019944221297,-0.213908268855235,
-2.59550682162745));
#5964=CARTESIAN_POINT('Ctrl Pts',(-26.8983181557808,-0.230051496944324,
-2.59360192011071));
#5965=CARTESIAN_POINT('Ctrl Pts',(-26.8902038146127,-0.262018183387908,
-2.58942059752268));
#5966=CARTESIAN_POINT('Ctrl Pts',(-26.8857646886985,-0.277849358655751,
-2.58714361859993));
#5967=CARTESIAN_POINT('Ctrl Pts',(-26.8713188216695,-0.324895801813619,
-2.57978251945632));
#5968=CARTESIAN_POINT('Ctrl Pts',(-26.8601834035885,-0.355670011650629,
-2.57416690219528));
#5969=CARTESIAN_POINT('Ctrl Pts',(-26.8412500664846,-0.400941255234936,
-2.56479529641425));
#5970=CARTESIAN_POINT('Ctrl Pts',(-26.8345604461981,-0.415894450482954,
-2.56151035689195));
#5971=CARTESIAN_POINT('Ctrl Pts',(-26.8239684235737,-0.43809039102524,-2.55636178150266));
#5972=CARTESIAN_POINT('Ctrl Pts',(-26.8203410661095,-0.445456832661156,
-2.55460695983524));
#5973=CARTESIAN_POINT('Ctrl Pts',(-26.8128999456829,-0.460110113434816,
-2.55102621846156));
#5974=CARTESIAN_POINT('Ctrl Pts',(-26.8090809400854,-0.467406099051344,
-2.54919783195028));
#5975=CARTESIAN_POINT('Ctrl Pts',(-26.7973956024953,-0.489075501379373,
-2.54363495988491));
#5976=CARTESIAN_POINT('Ctrl Pts',(-26.7892904087949,-0.503256366320303,
-2.53981745826163));
#5977=CARTESIAN_POINT('Ctrl Pts',(-26.7724556899274,-0.531115565582874,
-2.53198937867127));
#5978=CARTESIAN_POINT('Ctrl Pts',(-26.7637274203706,-0.544791910987859,
-2.52797935716389));
#5979=CARTESIAN_POINT('Ctrl Pts',(-26.7366217266702,-0.58507967901889,-2.51570272134658));
#5980=CARTESIAN_POINT('Ctrl Pts',(-26.7173257403855,-0.610951467196291,
-2.5071891514559));
#5981=CARTESIAN_POINT('Ctrl Pts',(-26.6865421652591,-0.648316199104958,
-2.49408756309349));
#5982=CARTESIAN_POINT('Ctrl Pts',(-26.6759737885839,-0.660530164014686,
-2.4896650790417));
#5983=CARTESIAN_POINT('Ctrl Pts',(-26.6542143618837,-0.68447654199776,-2.48073725881265));
#5984=CARTESIAN_POINT('Ctrl Pts',(-26.6430275831957,-0.696204572944766,
-2.47623358134868));
#5985=CARTESIAN_POINT('Ctrl Pts',(-26.625757459411,-0.713446061713053,-2.46943219638784));
#5986=CARTESIAN_POINT('Ctrl Pts',(-26.619921440287,-0.71913160109651,-2.46715852858782));
#5987=CARTESIAN_POINT('Ctrl Pts',(-26.6081492806517,-0.730323844266243,
-2.46262464724449));
#5988=CARTESIAN_POINT('Ctrl Pts',(-26.6022023493564,-0.735841448132365,
-2.4603601639289));
#5989=CARTESIAN_POINT('Ctrl Pts',(-26.5841990801845,-0.752142596351643,
-2.45358727585739));
#5990=CARTESIAN_POINT('Ctrl Pts',(-26.5719637153137,-0.762691293347727,
-2.44909283533732));
#5991=CARTESIAN_POINT('Ctrl Pts',(-26.5345859666616,-0.793375000104388,
-2.43572683396233));
#5992=CARTESIAN_POINT('Ctrl Pts',(-26.5087543078564,-0.812569281368951,
-2.42696429363964));
#5993=CARTESIAN_POINT('Ctrl Pts',(-26.4686216279805,-0.839484914822932,
-2.41422981442001));
#5994=CARTESIAN_POINT('Ctrl Pts',(-26.4550122677061,-0.848144060795981,
-2.41005301554825));
#5995=CARTESIAN_POINT('Ctrl Pts',(-26.4273198206187,-0.864833014186361,
-2.40186770943339));
#5996=CARTESIAN_POINT('Ctrl Pts',(-26.4132367723247,-0.872862861793055,
-2.39785915569382));
#5997=CARTESIAN_POINT('Ctrl Pts',(-26.3845827730249,-0.888283954759515,
-2.39004399122573));
#5998=CARTESIAN_POINT('Ctrl Pts',(-26.3700175910458,-0.895672296665481,
-2.38623887159212));
#5999=CARTESIAN_POINT('Ctrl Pts',(-26.3477725177819,-0.906273162875092,
-2.38070494715482));
#6000=CARTESIAN_POINT('Ctrl Pts',(-26.3402926727503,-0.909725000544915,
-2.37888997766033));
#6001=CARTESIAN_POINT('Ctrl Pts',(-26.3252947580114,-0.916423170547351,
-2.37534522135331));
#6002=CARTESIAN_POINT('Ctrl Pts',(-26.3177609641362,-0.919677618978278,
-2.37361127867653));
#6003=CARTESIAN_POINT('Ctrl Pts',(-26.279960326246,-0.935453358182183,-2.36515451304931));
#6004=CARTESIAN_POINT('Ctrl Pts',(-26.2492308175849,-0.946541064909447,
-2.35904578187963));
#6005=CARTESIAN_POINT('Ctrl Pts',(-26.1868089918217,-0.96567161724459,-2.34833908445429));
#6006=CARTESIAN_POINT('Ctrl Pts',(-26.1551127594127,-0.973718288717797,
-2.34373917694448));
#6007=CARTESIAN_POINT('Ctrl Pts',(-26.1068144462703,-0.983469972772359,
-2.33811102541251));
#6008=CARTESIAN_POINT('Ctrl Pts',(-26.090589178399,-0.986333510705604,-2.33644692696739));
#6009=CARTESIAN_POINT('Ctrl Pts',(-26.0578800212193,-0.991270124222091,
-2.33356672209884));
#6010=CARTESIAN_POINT('Ctrl Pts',(-26.0413989600866,-0.993342685095569,
-2.33235094950618));
#6011=CARTESIAN_POINT('Ctrl Pts',(-26.016468400417,-0.995843155056376,-2.33088062949275));
#6012=CARTESIAN_POINT('Ctrl Pts',(-26.0081137802036,-0.996575200948386,
-2.33044941555121));
#6013=CARTESIAN_POINT('Ctrl Pts',(-25.9914406456729,-0.997825328960477,
-2.32971229361946));
#6014=CARTESIAN_POINT('Ctrl Pts',(-25.9831090698346,-0.998345104091185,
-2.32940539355605));
#6015=CARTESIAN_POINT('Ctrl Pts',(-25.9581619918789,-0.999588413090816,
-2.32867085845433));
#6016=CARTESIAN_POINT('Ctrl Pts',(-25.9415535789236,-1.00000042873077,-2.32842685045339));
#6017=CARTESIAN_POINT('Ctrl Pts',(-25.8918801116584,-0.999999142511445,
-2.3284276733473));
#6018=CARTESIAN_POINT('Ctrl Pts',(-25.8588976369251,-0.998358102087351,
-2.32940162628821));
#6019=CARTESIAN_POINT('Ctrl Pts',(-25.809655452566,-0.993462469088689,-2.33228059590286));
#6020=CARTESIAN_POINT('Ctrl Pts',(-25.7932780679245,-0.991424398396009,
-2.3334763859153));
#6021=CARTESIAN_POINT('Ctrl Pts',(-25.7605967018549,-0.986531578876193,
-2.3363316707559));
#6022=CARTESIAN_POINT('Ctrl Pts',(-25.744287250752,-0.983675445441527,-2.33799197788889));
#6023=CARTESIAN_POINT('Ctrl Pts',(-25.7198948761487,-0.978775245710681,
-2.34082078278937));
#6024=CARTESIAN_POINT('Ctrl Pts',(-25.7117693154796,-0.97703729202741,-2.34182114664375));
#6025=CARTESIAN_POINT('Ctrl Pts',(-25.6955363910876,-0.973352864470024,
-2.34393407887513));
#6026=CARTESIAN_POINT('Ctrl Pts',(-25.6874340994824,-0.971407041360755,
-2.34504624803507));
#6027=CARTESIAN_POINT('Ctrl Pts',(-25.6632984183101,-0.965291239666667,
-2.34852759864218));
#6028=CARTESIAN_POINT('Ctrl Pts',(-25.6473893995262,-0.960834612092797,
-2.35104651772393));
#6029=CARTESIAN_POINT('Ctrl Pts',(-25.6159251530686,-0.951180080790836,
-2.35644914953995));
#6030=CARTESIAN_POINT('Ctrl Pts',(-25.6003693864664,-0.945982332371019,
-2.35933277792));
#6031=CARTESIAN_POINT('Ctrl Pts',(-25.5696010487147,-0.934857849827407,
-2.36543410266167));
#6032=CARTESIAN_POINT('Ctrl Pts',(-25.554388497757,-0.928931075544406,-2.36865182569907));
#6033=CARTESIAN_POINT('Ctrl Pts',(-25.5092553225566,-0.910065915709693,
-2.37876175430699));
#6034=CARTESIAN_POINT('Ctrl Pts',(-25.4798364380125,-0.896042727572783,
-2.38611169599139));
#6035=CARTESIAN_POINT('Ctrl Pts',(-25.4438909156586,-0.876699211680765,
-2.39591502278521));
#6036=CARTESIAN_POINT('Ctrl Pts',(-25.4367414461902,-0.872737300160875,
-2.39790741951297));
#6037=CARTESIAN_POINT('Ctrl Pts',(-25.4225293356803,-0.864633016249675,
-2.4019490228773));
#6038=CARTESIAN_POINT('Ctrl Pts',(-25.4154580969326,-0.860484766397168,
-2.40400099723934));
#6039=CARTESIAN_POINT('Ctrl Pts',(-25.3944657161042,-0.847820800232132,
-2.41021024122676));
#6040=CARTESIAN_POINT('Ctrl Pts',(-25.380746070164,-0.839077244133132,-2.41442548123447));
#6041=CARTESIAN_POINT('Ctrl Pts',(-25.3538260232817,-0.820989195886628,
-2.42297767676367));
#6042=CARTESIAN_POINT('Ctrl Pts',(-25.3406279393829,-0.811646297981063,
-2.42731389565942));
#6043=CARTESIAN_POINT('Ctrl Pts',(-25.3147430597672,-0.792367900936232,
-2.4360740734985));
#6044=CARTESIAN_POINT('Ctrl Pts',(-25.3020562810124,-0.782432389835531,
-2.44049806007426));
#6045=CARTESIAN_POINT('Ctrl Pts',(-25.2771860341754,-0.761968758341592,
-2.44940268163808));
#6046=CARTESIAN_POINT('Ctrl Pts',(-25.2650025732109,-0.751440637442869,
-2.45388334271683));
#6047=CARTESIAN_POINT('Ctrl Pts',(-25.2411353303519,-0.729786781206716,
-2.46287109582097));
#6048=CARTESIAN_POINT('Ctrl Pts',(-25.2294515461917,-0.718661056693565,
-2.46737821378511));
#6049=CARTESIAN_POINT('Ctrl Pts',(-25.2065843288473,-0.695801899103858,
-2.47638907712377));
#6050=CARTESIAN_POINT('Ctrl Pts',(-25.1954014188971,-0.684068711345196,
-2.48089267439044));
#6051=CARTESIAN_POINT('Ctrl Pts',(-25.1790045373378,-0.666000870018047,
-2.48762367211152));
#6052=CARTESIAN_POINT('Ctrl Pts',(-25.1735960376354,-0.659892776183962,
-2.48986579326022));
#6053=CARTESIAN_POINT('Ctrl Pts',(-25.1629494208789,-0.647568638488022,
-2.49431990834337));
#6054=CARTESIAN_POINT('Ctrl Pts',(-25.1577105174054,-0.641352897528938,
-2.49653204883514));
#6055=CARTESIAN_POINT('Ctrl Pts',(-25.1319358378313,-0.610000274169448,
-2.50751029184405));
#6056=CARTESIAN_POINT('Ctrl Pts',(-25.1126431635002,-0.584053957250262,
-2.51603030353833));
#6057=CARTESIAN_POINT('Ctrl Pts',(-25.0766559633797,-0.530429156133724,
-2.5323404528869));
#6058=CARTESIAN_POINT('Ctrl Pts',(-25.0599598863832,-0.5027512333643,-2.54013165293878));
#6059=CARTESIAN_POINT('Ctrl Pts',(-25.0368787132278,-0.459895387665408,
-2.55112212486567));
#6060=CARTESIAN_POINT('Ctrl Pts',(-25.0295127265205,-0.445386602515357,
-2.55466961647923));
#6061=CARTESIAN_POINT('Ctrl Pts',(-25.015447538885,-0.415909836891661,-2.56150652151534));
#6062=CARTESIAN_POINT('Ctrl Pts',(-25.0087479847154,-0.400940313195677,
-2.56479614450174));
#6063=CARTESIAN_POINT('Ctrl Pts',(-24.9992124578344,-0.378134446441367,
-2.56951620636083));
#6064=CARTESIAN_POINT('Ctrl Pts',(-24.9961153890925,-0.370461653972982,
-2.57105596109367));
#6065=CARTESIAN_POINT('Ctrl Pts',(-24.9901146400105,-0.355046096214791,
-2.57405082283813));
#6066=CARTESIAN_POINT('Ctrl Pts',(-24.9872162178828,-0.347318031889453,
-2.57550327285404));
#6067=CARTESIAN_POINT('Ctrl Pts',(-24.978823527118,-0.324069285671267,-2.57972387330155));
#6068=CARTESIAN_POINT('Ctrl Pts',(-24.9736218334904,-0.308462402151713,
-2.58236010535197));
#6069=CARTESIAN_POINT('Ctrl Pts',(-24.9640099750406,-0.277069749192375,
-2.58725894187428));
#6070=CARTESIAN_POINT('Ctrl Pts',(-24.9595973255169,-0.261278097086916,
-2.58952279476208));
#6071=CARTESIAN_POINT('Ctrl Pts',(-24.9515543557535,-0.229504132582814,
-2.59366790173024));
#6072=CARTESIAN_POINT('Ctrl Pts',(-24.9479240403419,-0.213521820083151,
-2.59554916744326));
#6073=CARTESIAN_POINT('Ctrl Pts',(-24.941447441202,-0.181365268356563,-2.59891718319403));
#6074=CARTESIAN_POINT('Ctrl Pts',(-24.9386011499407,-0.165191031604557,
-2.60040394522676));
#6075=CARTESIAN_POINT('Ctrl Pts',(-24.9337002237304,-0.132648091777223,
-2.60297035508352));
#6076=CARTESIAN_POINT('Ctrl Pts',(-24.93164556828,-0.116279393924668,-2.60405001587271));
#6077=CARTESIAN_POINT('Ctrl Pts',(-24.928341708171,-0.0833436511207354,
-2.60578872210514));
#6078=CARTESIAN_POINT('Ctrl Pts',(-24.9270927815557,-0.0667757724171859,
-2.60644761593104));
#6079=CARTESIAN_POINT('Ctrl Pts',(-24.9258378814317,-0.0417737140066712,
-2.60711000800062));
#6080=CARTESIAN_POINT('Ctrl Pts',(-24.9255229363957,-0.0334016706388513,
-2.60727635262695));
#6081=CARTESIAN_POINT('Ctrl Pts',(-24.9251040599288,-0.016674193542247,
-2.60749761997638));
#6082=CARTESIAN_POINT('Ctrl Pts',(-24.9249998216785,-0.00832709294464443,
-2.60755270409509));
#6083=CARTESIAN_POINT('Ctrl Pts',(-24.925,9.1987778071817E-16,-2.60755260924174));
#6084=CARTESIAN_POINT('',(-27.0987792489536,0.000111760644532478,-2.99999999791826));
#6085=CARTESIAN_POINT('',(-24.7512207470268,1.19503331376525E-15,-3.));
#6086=CARTESIAN_POINT('Ctrl Pts',(-27.0987792482096,0.000121760644497039,
-2.99999999752906));
#6087=CARTESIAN_POINT('Ctrl Pts',(-27.098788174959,-0.125283846590266,-3.00000466933289));
#6088=CARTESIAN_POINT('Ctrl Pts',(-27.0836572608919,-0.249887612487901,
-2.99204806120949));
#6089=CARTESIAN_POINT('Ctrl Pts',(-27.0242841101371,-0.489247948794867,
-2.96225146824176));
#6090=CARTESIAN_POINT('Ctrl Pts',(-26.9807678619009,-0.603149705373672,
-2.94076784698443));
#6091=CARTESIAN_POINT('Ctrl Pts',(-26.8427192011915,-0.860536585811288,
-2.87814965124282));
#6092=CARTESIAN_POINT('Ctrl Pts',(-26.7376907200788,-0.989566183854094,
-2.83419679721259));
#6093=CARTESIAN_POINT('Ctrl Pts',(-26.515546731998,-1.17588715226963,-2.76143949975895));
#6094=CARTESIAN_POINT('Ctrl Pts',(-26.4004065512224,-1.24404280001843,-2.73036038773096));
#6095=CARTESIAN_POINT('Ctrl Pts',(-26.1626806024214,-1.32927584783709,-2.68979319984398));
#6096=CARTESIAN_POINT('Ctrl Pts',(-26.0452468272229,-1.35044153732407,-2.6788631272028));
#6097=CARTESIAN_POINT('Ctrl Pts',(-25.8046235970334,-1.35043417397338,-2.67886683912841));
#6098=CARTESIAN_POINT('Ctrl Pts',(-25.6870707985623,-1.32923939483633,-2.68981328055134));
#6099=CARTESIAN_POINT('Ctrl Pts',(-25.4498537631474,-1.24407674422506,-2.73034115324496));
#6100=CARTESIAN_POINT('Ctrl Pts',(-25.3353287651251,-1.17639337787322,-2.76120614485257));
#6101=CARTESIAN_POINT('Ctrl Pts',(-25.1094606312527,-0.987455834848597,
-2.83506483214697));
#6102=CARTESIAN_POINT('Ctrl Pts',(-25.0061794065515,-0.857630793523992,
-2.87869860737191));
#6103=CARTESIAN_POINT('Ctrl Pts',(-24.8702787932849,-0.60571251075133,-2.94025713869714));
#6104=CARTESIAN_POINT('Ctrl Pts',(-24.826322397393,-0.491220877835279,-2.9619507002191));
#6105=CARTESIAN_POINT('Ctrl Pts',(-24.7664326588164,-0.250724694261063,
-2.9919992973031));
#6106=CARTESIAN_POINT('Ctrl Pts',(-24.7512189476652,-0.125688720919347,
-3.));
#6107=CARTESIAN_POINT('Ctrl Pts',(-24.7512207470268,1.27935820677023E-15,
-3.));
#6108=CARTESIAN_POINT('',(-26.9249999965755,8.27588207122033E-5,-2.60755260743232));
#6109=CARTESIAN_POINT('',(-27.0987792489536,0.000111760644532478,-2.99999999791826));
#6110=CARTESIAN_POINT('',(-26.925,-1.22464679914735E-16,-2.60755336253157));
#6111=CARTESIAN_POINT('Ctrl Pts',(-26.9249999965755,8.27588207122235E-5,
-2.60755260743232));
#6112=CARTESIAN_POINT('Ctrl Pts',(-26.9249999988585,5.51724988956825E-5,
-2.6075526086923));
#6113=CARTESIAN_POINT('Ctrl Pts',(-26.925,2.75862252984736E-5,-2.60755260934744));
#6114=CARTESIAN_POINT('Ctrl Pts',(-26.925,3.70771735314531E-16,-2.60755260939776));
#6115=CARTESIAN_POINT('',(-24.925,2.76064321768413E-16,-2.60755260924174));
#6116=CARTESIAN_POINT('Ctrl Pts',(-26.925,3.70771735314531E-16,-2.60755260939776));
#6117=CARTESIAN_POINT('Ctrl Pts',(-26.925,-0.0568048545755076,-2.60755271302726));
#6118=CARTESIAN_POINT('Ctrl Pts',(-26.9201545072348,-0.11340491023354,-2.60497728285413));
#6119=CARTESIAN_POINT('Ctrl Pts',(-26.9010104955459,-0.224986239203301,
-2.5949812948901));
#6120=CARTESIAN_POINT('Ctrl Pts',(-26.8867435237432,-0.279664869028174,
-2.58757303140778));
#6121=CARTESIAN_POINT('Ctrl Pts',(-26.8304379456036,-0.439261093144541,
-2.55919607531667));
#6122=CARTESIAN_POINT('Ctrl Pts',(-26.7755419497675,-0.537393100961328,
-2.53230699136511));
#6123=CARTESIAN_POINT('Ctrl Pts',(-26.6644533472358,-0.676591305065243,
-2.48451442941931));
#6124=CARTESIAN_POINT('Ctrl Pts',(-26.6171007671406,-0.724942488787085,
-2.46539574358496));
#6125=CARTESIAN_POINT('Ctrl Pts',(-26.4737133682738,-0.844473887402714,
-2.41369606443497));
#6126=CARTESIAN_POINT('Ctrl Pts',(-26.3682038617099,-0.904656958254231,
-2.3821133442928));
#6127=CARTESIAN_POINT('Ctrl Pts',(-26.1484453864063,-0.980999063110181,
-2.34001084161919));
#6128=CARTESIAN_POINT('Ctrl Pts',(-26.0378922085562,-1.00000218800714,-2.32842180399995));
#6129=CARTESIAN_POINT('Ctrl Pts',(-25.8119011916326,-0.999997808364594,
-2.3284324547047));
#6130=CARTESIAN_POINT('Ctrl Pts',(-25.701190289908,-0.980940359915226,-2.34004920952815));
#6131=CARTESIAN_POINT('Ctrl Pts',(-25.4813838789151,-0.904439026472573,
-2.38222657916128));
#6132=CARTESIAN_POINT('Ctrl Pts',(-25.3760142250185,-0.844278486742652,
-2.41378709535207));
#6133=CARTESIAN_POINT('Ctrl Pts',(-25.1812462928252,-0.681847452255133,
-2.48402790420274));
#6134=CARTESIAN_POINT('Ctrl Pts',(-25.0955604560339,-0.575048470588128,
-2.52290226852301));
#6135=CARTESIAN_POINT('Ctrl Pts',(-24.998457233114,-0.384117255242603,-2.56961701508285));
#6136=CARTESIAN_POINT('Ctrl Pts',(-24.9711794271723,-0.310565523100878,
-2.5835333593029));
#6137=CARTESIAN_POINT('Ctrl Pts',(-24.9343517093786,-0.157452571641774,
-2.60255728285361));
#6138=CARTESIAN_POINT('Ctrl Pts',(-24.925,-0.0790612261689355,-2.6075496863545));
#6139=CARTESIAN_POINT('Ctrl Pts',(-24.925,9.22656048785168E-16,-2.60755260924175));
#6140=CARTESIAN_POINT('',(-24.7512207470268,1.19503331376525E-15,-3.));
#6141=CARTESIAN_POINT('Ctrl Pts',(-24.7512205732181,-1.76183185122132E-16,
3.00000039251396));
#6142=CARTESIAN_POINT('Ctrl Pts',(-24.7512209918384,-0.0224904489448875,
3.0000001742556));
#6143=CARTESIAN_POINT('Ctrl Pts',(-24.7517089574441,-0.0449130845232464,
2.99974733834206));
#6144=CARTESIAN_POINT('Ctrl Pts',(-24.7536443519837,-0.0895752381506375,
2.99874599882652));
#6145=CARTESIAN_POINT('Ctrl Pts',(-24.7550914179306,-0.111823200513362,
2.9979976955573));
#6146=CARTESIAN_POINT('Ctrl Pts',(-24.7608544959128,-0.178320919528189,
2.99502476849759));
#6147=CARTESIAN_POINT('Ctrl Pts',(-24.766591932863,-0.222335186723983,2.99207096785045));
#6148=CARTESIAN_POINT('Ctrl Pts',(-24.7780291872986,-0.287837198516676,
2.98624078109657));
#6149=CARTESIAN_POINT('Ctrl Pts',(-24.7823200974485,-0.30960638724731,2.98406110217344));
#6150=CARTESIAN_POINT('Ctrl Pts',(-24.789468342319,-0.342109605994453,2.98045008409494));
#6151=CARTESIAN_POINT('Ctrl Pts',(-24.7919728029526,-0.352929856681446,
2.97918798270959));
#6152=CARTESIAN_POINT('Ctrl Pts',(-24.7972217651647,-0.37452313010145,2.97655057002885));
#6153=CARTESIAN_POINT('Ctrl Pts',(-24.7999685317995,-0.385302680101395,
2.97517414639763));
#6154=CARTESIAN_POINT('Ctrl Pts',(-24.8085250872429,-0.41739609024285,2.97090016875934));
#6155=CARTESIAN_POINT('Ctrl Pts',(-24.81466151752,-0.438519418189051,2.96785256118554));
#6156=CARTESIAN_POINT('Ctrl Pts',(-24.8277811472732,-0.480245335622268,
2.96138693176614));
#6157=CARTESIAN_POINT('Ctrl Pts',(-24.8347637590013,-0.500846703560905,
2.95796918269451));
#6158=CARTESIAN_POINT('Ctrl Pts',(-24.8569589172265,-0.561884990270968,
2.94720128262928));
#6159=CARTESIAN_POINT('Ctrl Pts',(-24.8734161226417,-0.601558077547717,
2.93933624108072));
#6160=CARTESIAN_POINT('Ctrl Pts',(-24.9005702937365,-0.65957757549401,2.92666224804854));
#6161=CARTESIAN_POINT('Ctrl Pts',(-24.9100346262345,-0.678669948505794,
2.9222910240135));
#6162=CARTESIAN_POINT('Ctrl Pts',(-24.9297928233973,-0.716355649282141,
2.91328208432799));
#6163=CARTESIAN_POINT('Ctrl Pts',(-24.9400945131254,-0.734962441112178,
2.90864084409791));
#6164=CARTESIAN_POINT('Ctrl Pts',(-24.961514660095,-0.77162967400038,2.89912896911718));
#6165=CARTESIAN_POINT('Ctrl Pts',(-24.9725545674253,-0.789557946478675,
2.89429319601545));
#6166=CARTESIAN_POINT('Ctrl Pts',(-24.9953084665056,-0.824674949037347,
2.88448368582705));
#6167=CARTESIAN_POINT('Ctrl Pts',(-25.0070179507415,-0.841855856812551,
2.87951192539658));
#6168=CARTESIAN_POINT('Ctrl Pts',(-25.043133571216,-0.892292847196549,2.86444548622589));
#6169=CARTESIAN_POINT('Ctrl Pts',(-25.0685243392037,-0.924445728200638,
2.85419906644615));
#6170=CARTESIAN_POINT('Ctrl Pts',(-25.1085920152708,-0.970518787083053,
2.83872479371573));
#6171=CARTESIAN_POINT('Ctrl Pts',(-25.1222787941031,-0.985516398208712,
2.83354919922538));
#6172=CARTESIAN_POINT('Ctrl Pts',(-25.1503247573348,-1.01479098932509,2.82319728666854));
#6173=CARTESIAN_POINT('Ctrl Pts',(-25.164690788982,-1.02907375849125,2.81801865872127));
#6174=CARTESIAN_POINT('Ctrl Pts',(-25.1940841805899,-1.05688925756544,2.80770519124119));
#6175=CARTESIAN_POINT('Ctrl Pts',(-25.2091790647757,-1.07047808243068,2.80254833483866));
#6176=CARTESIAN_POINT('Ctrl Pts',(-25.2397860183817,-1.09666813400313,2.79240366726727));
#6177=CARTESIAN_POINT('Ctrl Pts',(-25.2553204379955,-1.1092959595929,2.78740689519965));
#6178=CARTESIAN_POINT('Ctrl Pts',(-25.2868471218303,-1.13362876731755,2.7775997880586));
#6179=CARTESIAN_POINT('Ctrl Pts',(-25.3028398226619,-1.1453347251136,2.77278915814535));
#6180=CARTESIAN_POINT('Ctrl Pts',(-25.3352862383422,-1.16783527307201,2.7633878040888));
#6181=CARTESIAN_POINT('Ctrl Pts',(-25.351739959153,-1.17862983581216,2.75879704618161));
#6182=CARTESIAN_POINT('Ctrl Pts',(-25.4018015943325,-1.20964925021433,2.74540688876099));
#6183=CARTESIAN_POINT('Ctrl Pts',(-25.4361159534219,-1.22851653432304,2.73698721829838));
#6184=CARTESIAN_POINT('Ctrl Pts',(-25.4890321005069,-1.2540267758302,2.72534532216722));
#6185=CARTESIAN_POINT('Ctrl Pts',(-25.5069295704027,-1.26207047477092,2.72162643380116));
#6186=CARTESIAN_POINT('Ctrl Pts',(-25.5341342320122,-1.2734140814595,2.71632781873948));
#6187=CARTESIAN_POINT('Ctrl Pts',(-25.5432728261675,-1.27707857798256,2.71460649012168));
#6188=CARTESIAN_POINT('Ctrl Pts',(-25.5616697300355,-1.2841624728764,2.71126260047887));
#6189=CARTESIAN_POINT('Ctrl Pts',(-25.5709428123064,-1.28758661927441,2.70963775628573));
#6190=CARTESIAN_POINT('Ctrl Pts',(-25.5987921995341,-1.29743171221407,2.7049448162659));
#6191=CARTESIAN_POINT('Ctrl Pts',(-25.6174339809943,-1.3034429040471,2.70205039524382));
#6192=CARTESIAN_POINT('Ctrl Pts',(-25.6548880488268,-1.31438298806204,2.69674565415259));
#6193=CARTESIAN_POINT('Ctrl Pts',(-25.6736969296858,-1.31931098956042,2.69433575157958));
#6194=CARTESIAN_POINT('Ctrl Pts',(-25.7303690862317,-1.33248199267997,2.68785983771893));
#6195=CARTESIAN_POINT('Ctrl Pts',(-25.7684774334826,-1.33911568210638,2.68454786410377));
#6196=CARTESIAN_POINT('Ctrl Pts',(-25.8261391530629,-1.34582335222856,2.6811878846237));
#6197=CARTESIAN_POINT('Ctrl Pts',(-25.8454430323917,-1.34751786899546,2.6803358118198));
#6198=CARTESIAN_POINT('Ctrl Pts',(-25.8842203925786,-1.34980777647361,2.67918335088873));
#6199=CARTESIAN_POINT('Ctrl Pts',(-25.903705143976,-1.35040245497255,2.67888335709825));
#6200=CARTESIAN_POINT('Ctrl Pts',(-25.9428031383705,-1.3504709734195,2.67884881443484));
#6201=CARTESIAN_POINT('Ctrl Pts',(-25.9625262668505,-1.34993687451433,2.67911827983488));
#6202=CARTESIAN_POINT('Ctrl Pts',(-26.0016751544636,-1.34774181046254,2.68022319148998));
#6203=CARTESIAN_POINT('Ctrl Pts',(-26.0211401155725,-1.34608678179488,2.68105562372842));
#6204=CARTESIAN_POINT('Ctrl Pts',(-26.059852112923,-1.34168298980989,2.68326212736971));
#6205=CARTESIAN_POINT('Ctrl Pts',(-26.0790998997345,-1.3389348308238,2.68463587910206));
#6206=CARTESIAN_POINT('Ctrl Pts',(-26.1173832113779,-1.3323621027606,2.6879039252919));
#6207=CARTESIAN_POINT('Ctrl Pts',(-26.1364187282489,-1.32853748653121,2.68979822524671));
#6208=CARTESIAN_POINT('Ctrl Pts',(-26.1932111473027,-1.31546058553577,2.69623084419525));
#6209=CARTESIAN_POINT('Ctrl Pts',(-26.2306587701737,-1.30460495425468,2.70152087608487));
#6210=CARTESIAN_POINT('Ctrl Pts',(-26.2769393229609,-1.28835507017719,2.70927245589678));
#6211=CARTESIAN_POINT('Ctrl Pts',(-26.2861735714613,-1.28496732277493,2.7108812019877));
#6212=CARTESIAN_POINT('Ctrl Pts',(-26.3045800008344,-1.27792560939944,2.71420782302654));
#6213=CARTESIAN_POINT('Ctrl Pts',(-26.3137695365298,-1.27426364167247,2.71592937831153));
#6214=CARTESIAN_POINT('Ctrl Pts',(-26.3411342135086,-1.26291934373526,2.72123265364054));
#6215=CARTESIAN_POINT('Ctrl Pts',(-26.359108489593,-1.25488165967842,2.72495179584752));
#6216=CARTESIAN_POINT('Ctrl Pts',(-26.3945729485003,-1.23786371810422,2.73272458713573));
#6217=CARTESIAN_POINT('Ctrl Pts',(-26.4120572689161,-1.22888610491339,2.73677701321046));
#6218=CARTESIAN_POINT('Ctrl Pts',(-26.4465442238038,-1.21000802381102,2.74517577574546));
#6219=CARTESIAN_POINT('Ctrl Pts',(-26.4635468416444,-1.20010753017731,2.74952213668882));
#6220=CARTESIAN_POINT('Ctrl Pts',(-26.4970804298005,-1.17938992628659,2.75847230162352));
#6221=CARTESIAN_POINT('Ctrl Pts',(-26.5136113919084,-1.16857280798542,2.76307612855274));
#6222=CARTESIAN_POINT('Ctrl Pts',(-26.5462078840406,-1.14602038731631,2.77250596727389));
#6223=CARTESIAN_POINT('Ctrl Pts',(-26.562273493867,-1.1342850254395,2.7773320282384));
#6224=CARTESIAN_POINT('Ctrl Pts',(-26.5939414283119,-1.1098870091199,2.78717177677759));
#6225=CARTESIAN_POINT('Ctrl Pts',(-26.6095473445416,-1.09722131473955,2.79218666030944));
#6226=CARTESIAN_POINT('Ctrl Pts',(-26.6402811143626,-1.07095661488449,2.8023656091679));
#6227=CARTESIAN_POINT('Ctrl Pts',(-26.6552948463125,-1.0574557506976,2.80749156457345));
#6228=CARTESIAN_POINT('Ctrl Pts',(-26.6846546110444,-1.02971343125001,2.817784903976));
#6229=CARTESIAN_POINT('Ctrl Pts',(-26.6989977054847,-1.0154744409772,2.82295134426973));
#6230=CARTESIAN_POINT('Ctrl Pts',(-26.7270250638549,-0.98626566630943,2.83328830718172));
#6231=CARTESIAN_POINT('Ctrl Pts',(-26.7407092830319,-0.971295850373591,
2.83845888576662));
#6232=CARTESIAN_POINT('Ctrl Pts',(-26.7807869864753,-0.925288343298035,
2.85392552592912));
#6233=CARTESIAN_POINT('Ctrl Pts',(-26.8062104528913,-0.893151438987829,
2.86417785822885));
#6234=CARTESIAN_POINT('Ctrl Pts',(-26.8423944800688,-0.842704105273581,
2.87926390500452));
#6235=CARTESIAN_POINT('Ctrl Pts',(-26.854135591242,-0.825504489114962,2.88424645343755));
#6236=CARTESIAN_POINT('Ctrl Pts',(-26.8712462612575,-0.799138658144533,
2.89161951102431));
#6237=CARTESIAN_POINT('Ctrl Pts',(-26.876870779104,-0.790247883055737,2.89406240563577));
#6238=CARTESIAN_POINT('Ctrl Pts',(-26.8879469072246,-0.772281655830627,
2.89890846334945));
#6239=CARTESIAN_POINT('Ctrl Pts',(-26.893409269784,-0.763187520111312,2.90131641792487));
#6240=CARTESIAN_POINT('Ctrl Pts',(-26.9094749238114,-0.735724555729972,
2.90844791977076));
#6241=CARTESIAN_POINT('Ctrl Pts',(-26.9197549867311,-0.717184843056228,
2.91307769758814));
#6242=CARTESIAN_POINT('Ctrl Pts',(-26.9394913365264,-0.679605859000123,
2.92207317082987));
#6243=CARTESIAN_POINT('Ctrl Pts',(-26.9489438557812,-0.660573303647308,
2.92643722327291));
#6244=CARTESIAN_POINT('Ctrl Pts',(-26.9760661551845,-0.602745633656236,
2.93909124911831));
#6245=CARTESIAN_POINT('Ctrl Pts',(-26.9925036507446,-0.563222175536769,
2.94694362837257));
#6246=CARTESIAN_POINT('Ctrl Pts',(-27.0220715762404,-0.482184664459269,
2.96128235245645));
#6247=CARTESIAN_POINT('Ctrl Pts',(-27.0352035249924,-0.440658030285012,
2.96777002657001));
#6248=CARTESIAN_POINT('Ctrl Pts',(-27.0523216883035,-0.376833839229866,
2.97631699067074));
#6249=CARTESIAN_POINT('Ctrl Pts',(-27.0576005303158,-0.355274412887369,
2.97897027612799));
#6250=CARTESIAN_POINT('Ctrl Pts',(-27.0672600591522,-0.311662753136127,
2.98384821443584));
#6251=CARTESIAN_POINT('Ctrl Pts',(-27.0716114828177,-0.289741794867057,
2.9860580250039));
#6252=CARTESIAN_POINT('Ctrl Pts',(-27.0793660357628,-0.245626078050731,
2.99001014183974));
#6253=CARTESIAN_POINT('Ctrl Pts',(-27.0827661298392,-0.223449095191076,
2.99175090619715));
#6254=CARTESIAN_POINT('Ctrl Pts',(-27.088612570746,-0.178789136156301,2.99475173451271));
#6255=CARTESIAN_POINT('Ctrl Pts',(-27.0910448696872,-0.1564046715903,2.99600458388059));
#6256=CARTESIAN_POINT('Ctrl Pts',(-27.096853679446,-0.0893800225646477,
2.9990010619891));
#6257=CARTESIAN_POINT('Ctrl Pts',(-27.098776248484,-0.0447217666279726,
2.99999873125252));
#6258=CARTESIAN_POINT('Ctrl Pts',(-27.0987810099015,0.0221932423036746,
3.00000122002206));
#6259=CARTESIAN_POINT('Ctrl Pts',(-27.0983026039981,0.0444881794306487,
2.99975332625577));
#6260=CARTESIAN_POINT('Ctrl Pts',(-27.0963847740834,0.0890579105479431,
2.99876106205554));
#6261=CARTESIAN_POINT('Ctrl Pts',(-27.0949453773135,0.111332705013246,2.99801669216856));
#6262=CARTESIAN_POINT('Ctrl Pts',(-27.0910975380372,0.155862012281645,2.99603172453301));
#6263=CARTESIAN_POINT('Ctrl Pts',(-27.0886879051299,0.178121225730192,2.99479051237394));
#6264=CARTESIAN_POINT('Ctrl Pts',(-27.0828889596371,0.222600296296532,2.99181384430896));
#6265=CARTESIAN_POINT('Ctrl Pts',(-27.0794840506901,0.244888396742269,2.99007048023225));
#6266=CARTESIAN_POINT('Ctrl Pts',(-27.071775952777,0.288869899263917,2.98614166251469));
#6267=CARTESIAN_POINT('Ctrl Pts',(-27.0674608269688,0.310670331278556,2.98395006519914));
#6268=CARTESIAN_POINT('Ctrl Pts',(-27.0579363802439,0.353839366034685,2.9791394357373));
#6269=CARTESIAN_POINT('Ctrl Pts',(-27.0527258255725,0.375218389994932,2.97651976178013));
#6270=CARTESIAN_POINT('Ctrl Pts',(-27.0357695640527,0.438751704381788,2.96805078583667));
#6271=CARTESIAN_POINT('Ctrl Pts',(-27.0226990393997,0.48031037316965,2.96158999423889));
#6272=CARTESIAN_POINT('Ctrl Pts',(-27.0004754778274,0.541446390227552,2.95080792183841));
#6273=CARTESIAN_POINT('Ctrl Pts',(-26.9926233391618,0.561639756422948,2.94702858491465));
#6274=CARTESIAN_POINT('Ctrl Pts',(-26.9801906409175,0.5916140025928,2.94110512698185));
#6275=CARTESIAN_POINT('Ctrl Pts',(-26.9759329233523,0.601561926835117,2.9390861971729));
#6276=CARTESIAN_POINT('Ctrl Pts',(-26.9671986892834,0.621350277064186,2.93496653895837));
#6277=CARTESIAN_POINT('Ctrl Pts',(-26.9627160190823,0.631203054805755,2.93286297248301));
#6278=CARTESIAN_POINT('Ctrl Pts',(-26.949000010224,0.660466243653672,2.92646286445819));
#6279=CARTESIAN_POINT('Ctrl Pts',(-26.9394863006083,0.679616625492281,2.92207081256718));
#6280=CARTESIAN_POINT('Ctrl Pts',(-26.9197260539462,0.717238752620466,2.91306457362862));
#6281=CARTESIAN_POINT('Ctrl Pts',(-26.9094809907086,0.7357078120015,2.90845102679016));
#6282=CARTESIAN_POINT('Ctrl Pts',(-26.8776648850953,0.790113953263617,2.8943267049494));
#6283=CARTESIAN_POINT('Ctrl Pts',(-26.8550156533739,0.825052204528997,2.88453180649776));
#6284=CARTESIAN_POINT('Ctrl Pts',(-26.8188825262082,0.875510966128809,2.86945837323707));
#6285=CARTESIAN_POINT('Ctrl Pts',(-26.8064775830923,0.892005171014219,2.86437028648305));
#6286=CARTESIAN_POINT('Ctrl Pts',(-26.7809368156929,0.92434327478541,2.85409879125165));
#6287=CARTESIAN_POINT('Ctrl Pts',(-26.767806005017,0.940181255880788,2.8489172911309));
#6288=CARTESIAN_POINT('Ctrl Pts',(-26.7475346890206,0.963464821076118,2.84109226874023));
#6289=CARTESIAN_POINT('Ctrl Pts',(-26.7406844898386,0.971142790692541,2.83847640424403));
#6290=CARTESIAN_POINT('Ctrl Pts',(-26.7268665710498,0.986257223502056,2.83326015443131));
#6291=CARTESIAN_POINT('Ctrl Pts',(-26.7198861854429,0.993708406579356,2.83065485672359));
#6292=CARTESIAN_POINT('Ctrl Pts',(-26.6987543184742,1.01572209996892,2.82286262012559));
#6293=CARTESIAN_POINT('Ctrl Pts',(-26.6843926989096,1.02996746343674,2.81769174714818));
#6294=CARTESIAN_POINT('Ctrl Pts',(-26.6405194665222,1.07140391340386,2.80231410558904));
#6295=CARTESIAN_POINT('Ctrl Pts',(-26.6101987968579,1.09732460419766,2.79223276559478));
#6296=CARTESIAN_POINT('Ctrl Pts',(-26.5630918828768,1.13367250400702,2.77758169296716));
#6297=CARTESIAN_POINT('Ctrl Pts',(-26.5471174957754,1.14536614557726,2.7727762680603));
#6298=CARTESIAN_POINT('Ctrl Pts',(-26.514612671107,1.16790354588699,2.76335903848249));
#6299=CARTESIAN_POINT('Ctrl Pts',(-26.4980822787532,1.17874735889937,2.7587471803173));
#6300=CARTESIAN_POINT('Ctrl Pts',(-26.46444880388,1.19957259205024,2.74975580028195));
#6301=CARTESIAN_POINT('Ctrl Pts',(-26.4473524929256,1.20955009125368,2.74537799392286));
#6302=CARTESIAN_POINT('Ctrl Pts',(-26.4212416835811,1.22386590602098,2.73901119026752));
#6303=CARTESIAN_POINT('Ctrl Pts',(-26.4124619953677,1.22852739949808,2.73692306012723));
#6304=CARTESIAN_POINT('Ctrl Pts',(-26.3948577516024,1.23757286419293,2.73284480288515));
#6305=CARTESIAN_POINT('Ctrl Pts',(-26.3860147393496,1.2419677956983,2.73084989444486));
#6306=CARTESIAN_POINT('Ctrl Pts',(-26.3416451282571,1.26327195668703,2.72112034953697));
#6307=CARTESIAN_POINT('Ctrl Pts',(-26.3055754632133,1.27824521948246,2.71409222828943));
#6308=CARTESIAN_POINT('Ctrl Pts',(-26.2323060083433,1.30407984829821,2.70177412725945));
#6309=CARTESIAN_POINT('Ctrl Pts',(-26.1951016228418,1.31494638090081,2.69648191406169));
#6310=CARTESIAN_POINT('Ctrl Pts',(-26.1384100565222,1.3281154276414,2.69000670173171));
#6311=CARTESIAN_POINT('Ctrl Pts',(-26.1193651709025,1.33198245867611,2.68809214937698));
#6312=CARTESIAN_POINT('Ctrl Pts',(-26.0809718351375,1.33864905018687,2.68477846139787));
#6313=CARTESIAN_POINT('Ctrl Pts',(-26.0616267046488,1.34144791557871,2.68337970984735));
#6314=CARTESIAN_POINT('Ctrl Pts',(-26.0323637266099,1.34482464575181,2.68168810040418));
#6315=CARTESIAN_POINT('Ctrl Pts',(-26.0225572452852,1.34581322849437,2.68119198692629));
#6316=CARTESIAN_POINT('Ctrl Pts',(-26.0029866629929,1.34750144912674,2.68034392500147));
#6317=CARTESIAN_POINT('Ctrl Pts',(-25.993207230682,1.34820337332278,2.67999083517032));
#6318=CARTESIAN_POINT('Ctrl Pts',(-25.9639248638171,1.34988238530037,2.67914574940457));
#6319=CARTESIAN_POINT('Ctrl Pts',(-25.944430250381,1.35043878696276,2.67886501715933));
#6320=CARTESIAN_POINT('Ctrl Pts',(-25.8861245564454,1.35043705000303,2.67886596390228));
#6321=CARTESIAN_POINT('Ctrl Pts',(-25.8474104061639,1.34822092631381,2.67998650091244));
#6322=CARTESIAN_POINT('Ctrl Pts',(-25.7896109432291,1.34160967645963,2.68329876772693));
#6323=CARTESIAN_POINT('Ctrl Pts',(-25.7703875060739,1.33885738792583,2.68467452923362));
#6324=CARTESIAN_POINT('Ctrl Pts',(-25.7320267909422,1.33224993750147,2.68795954661436));
#6325=CARTESIAN_POINT('Ctrl Pts',(-25.7128830927771,1.32839290578458,2.68986973704837));
#6326=CARTESIAN_POINT('Ctrl Pts',(-25.684251825295,1.32177548884068,2.69312428914529));
#6327=CARTESIAN_POINT('Ctrl Pts',(-25.6747142093514,1.31942848978327,2.69427521202406));
#6328=CARTESIAN_POINT('Ctrl Pts',(-25.6556603366635,1.31445289803521,2.6967061495634));
#6329=CARTESIAN_POINT('Ctrl Pts',(-25.6461500334678,1.31182518416256,2.69798570492286));
#6330=CARTESIAN_POINT('Ctrl Pts',(-25.6178200674555,1.30356617188208,2.70199101363685));
#6331=CARTESIAN_POINT('Ctrl Pts',(-25.5991463885073,1.2975477717278,2.70488904077814));
#6332=CARTESIAN_POINT('Ctrl Pts',(-25.5622143033361,1.28450992377734,2.711104791713));
#6333=CARTESIAN_POINT('Ctrl Pts',(-25.5439552645306,1.27749068571576,2.7144224184567));
#6334=CARTESIAN_POINT('Ctrl Pts',(-25.5078400226815,1.26246775944474,2.72144201858098));
#6335=CARTESIAN_POINT('Ctrl Pts',(-25.4899838433394,1.25446401700334,2.72514402265193));
#6336=CARTESIAN_POINT('Ctrl Pts',(-25.4370074508209,1.22898778436132,2.736775538613));
#6337=CARTESIAN_POINT('Ctrl Pts',(-25.402476169391,1.21005033530758,2.74523167785092));
#6338=CARTESIAN_POINT('Ctrl Pts',(-25.3602840547609,1.18392811236616,2.75651044711871));
#6339=CARTESIAN_POINT('Ctrl Pts',(-25.3518921545878,1.17857779567387,2.75880270804698));
#6340=CARTESIAN_POINT('Ctrl Pts',(-25.33521027166,1.16763346103172,2.76345258994632));
#6341=CARTESIAN_POINT('Ctrl Pts',(-25.3269101970962,1.16203150593468,2.76581339519711));
#6342=CARTESIAN_POINT('Ctrl Pts',(-25.3022697723606,1.14492960216065,2.77295715687365));
#6343=CARTESIAN_POINT('Ctrl Pts',(-25.2861659342133,1.13312196993095,2.77780680847141));
#6344=CARTESIAN_POINT('Ctrl Pts',(-25.2545677370148,1.10869517847092,2.78764614588441));
#6345=CARTESIAN_POINT('Ctrl Pts',(-25.2390760976615,1.09607817216592,2.79263498420858));
#6346=CARTESIAN_POINT('Ctrl Pts',(-25.2086929585038,1.0700438882078,2.80271360615569));
#6347=CARTESIAN_POINT('Ctrl Pts',(-25.1938014786094,1.05662659440153,2.80780342156985));
#6348=CARTESIAN_POINT('Ctrl Pts',(-25.1646092945331,1.02899172455791,2.81804822663801));
#6349=CARTESIAN_POINT('Ctrl Pts',(-25.1503085987059,1.01477414783796,2.82320324630945));
#6350=CARTESIAN_POINT('Ctrl Pts',(-25.122293720064,0.985531953026374,2.83354369456913));
#6351=CARTESIAN_POINT('Ctrl Pts',(-25.1085795345898,0.970507349552267,2.83872915299999));
#6352=CARTESIAN_POINT('Ctrl Pts',(-25.0817384653232,0.939637469740702,2.84909618968299));
#6353=CARTESIAN_POINT('Ctrl Pts',(-25.0686121956922,0.923792524689849,2.85427759753642));
#6354=CARTESIAN_POINT('Ctrl Pts',(-25.0493658734545,0.899393021425867,2.86202163910769));
#6355=CARTESIAN_POINT('Ctrl Pts',(-25.043017487774,0.891144418134318,2.86460120904708));
#6356=CARTESIAN_POINT('Ctrl Pts',(-25.0305207080604,0.874501431709212,2.86972568743743));
#6357=CARTESIAN_POINT('Ctrl Pts',(-25.0243713909441,0.866107457626742,2.87227076450331));
#6358=CARTESIAN_POINT('Ctrl Pts',(-24.9941176023294,0.823767677123202,2.88490127988302));
#6359=CARTESIAN_POINT('Ctrl Pts',(-24.97147225811,0.788728779396098,2.89470358965755));
#6360=CARTESIAN_POINT('Ctrl Pts',(-24.9292312229828,0.716311799075428,2.9134684860099));
#6361=CARTESIAN_POINT('Ctrl Pts',(-24.9096337112948,0.67893447464684,2.92243229488295));
#6362=CARTESIAN_POINT('Ctrl Pts',(-24.8825415051001,0.621060303181761,2.93507687968496));
#6363=CARTESIAN_POINT('Ctrl Pts',(-24.8738954614447,0.601467085362858,2.93915828390893));
#6364=CARTESIAN_POINT('Ctrl Pts',(-24.8573860335644,0.561660534816686,2.94702417229759));
#6365=CARTESIAN_POINT('Ctrl Pts',(-24.8495222347111,0.541445118061444,2.95080889756673));
#6366=CARTESIAN_POINT('Ctrl Pts',(-24.8383296294352,0.510647204231347,2.95623934885628));
#6367=CARTESIAN_POINT('Ctrl Pts',(-24.8346943538624,0.500285572119667,2.95801084324021));
#6368=CARTESIAN_POINT('Ctrl Pts',(-24.8276507980447,0.479467813925561,2.96145644444383));
#6369=CARTESIAN_POINT('Ctrl Pts',(-24.8242486897808,0.469031540585877,2.96312749437884));
#6370=CARTESIAN_POINT('Ctrl Pts',(-24.8143975220266,0.437635545407865,2.967983313185));
#6371=CARTESIAN_POINT('Ctrl Pts',(-24.8082918810615,0.41655941359351,2.97101630939715));
#6372=CARTESIAN_POINT('Ctrl Pts',(-24.79700967936,0.374165575587154,2.97665244169902));
#6373=CARTESIAN_POINT('Ctrl Pts',(-24.7918302021315,0.352839925216633,2.97925701409689));
#6374=CARTESIAN_POINT('Ctrl Pts',(-24.782389529693,0.309931149531077,2.98402597733368));
#6375=CARTESIAN_POINT('Ctrl Pts',(-24.7781283401501,0.288348024079468,2.98619038155605));
#6376=CARTESIAN_POINT('Ctrl Pts',(-24.7705262413241,0.244922587990788,2.99006529803462));
#6377=CARTESIAN_POINT('Ctrl Pts',(-24.767185323199,0.223080280695768,2.9917758240911));
#6378=CARTESIAN_POINT('Ctrl Pts',(-24.7614327168412,0.179133051352736,2.99472848957151));
#6379=CARTESIAN_POINT('Ctrl Pts',(-24.7590210045444,0.157028136357561,2.9959706439119));
#6380=CARTESIAN_POINT('Ctrl Pts',(-24.7551430015195,0.112550450866727,2.99797103284412));
#6381=CARTESIAN_POINT('Ctrl Pts',(-24.7536770371529,0.0901765544388111,
2.99872909299962));
#6382=CARTESIAN_POINT('Ctrl Pts',(-24.7522040612047,0.056412819484831,2.9994911778993));
#6383=CARTESIAN_POINT('Ctrl Pts',(-24.7518343852008,0.0451068922413156,
2.999682558101));
#6384=CARTESIAN_POINT('Ctrl Pts',(-24.7513427166217,0.0225174680468748,
2.99993712712975));
#6385=CARTESIAN_POINT('Ctrl Pts',(-24.7512203639079,0.0112452244724433,
3.00000050164314));
#6386=CARTESIAN_POINT('Ctrl Pts',(-24.7512205732181,-1.76183185122132E-16,
3.00000039251396));
#6387=CARTESIAN_POINT('Ctrl Pts',(-24.925,1.55854062294791E-16,2.60755260924175));
#6388=CARTESIAN_POINT('Ctrl Pts',(-24.9250003566431,-0.0166541858892895,
2.60755241953505));
#6389=CARTESIAN_POINT('Ctrl Pts',(-24.9254160783661,-0.0332581559508135,
2.60733265858179));
#6390=CARTESIAN_POINT('Ctrl Pts',(-24.9270649354643,-0.0663304974791156,
2.60646231020683));
#6391=CARTESIAN_POINT('Ctrl Pts',(-24.9282977615931,-0.0828051219601001,
2.60581189691127));
#6392=CARTESIAN_POINT('Ctrl Pts',(-24.9332076090917,-0.132046707858214,
2.60322787601199));
#6393=CARTESIAN_POINT('Ctrl Pts',(-24.9380956117425,-0.164639289236404,
2.6006604794867));
#6394=CARTESIAN_POINT('Ctrl Pts',(-24.9478395671871,-0.213143553563254,
2.59559297392188));
#6395=CARTESIAN_POINT('Ctrl Pts',(-24.9514952030343,-0.229263645988799,
2.59369843168223));
#6396=CARTESIAN_POINT('Ctrl Pts',(-24.9575851418319,-0.253332291674963,
2.59055979222183));
#6397=CARTESIAN_POINT('Ctrl Pts',(-24.9597188141185,-0.261344691370318,
2.58946279377859));
#6398=CARTESIAN_POINT('Ctrl Pts',(-24.9641906612921,-0.277334518444499,
2.58717039663941));
#6399=CARTESIAN_POINT('Ctrl Pts',(-24.966530765891,-0.285316779266169,2.58597403111897));
#6400=CARTESIAN_POINT('Ctrl Pts',(-24.973820513222,-0.309081961524915,2.58225915775743));
#6401=CARTESIAN_POINT('Ctrl Pts',(-24.9790484377681,-0.324723793798948,
2.57961022574372));
#6402=CARTESIAN_POINT('Ctrl Pts',(-24.9902256908821,-0.355621851323135,
2.57399040352469));
#6403=CARTESIAN_POINT('Ctrl Pts',(-24.9961745187184,-0.37087717201515,2.57101975041036));
#6404=CARTESIAN_POINT('Ctrl Pts',(-25.0150836576248,-0.416076046241271,
2.5616604629974));
#6405=CARTESIAN_POINT('Ctrl Pts',(-25.0291043543913,-0.445453982261499,
2.5548242940218));
#6406=CARTESIAN_POINT('Ctrl Pts',(-25.0522383184702,-0.488417442273932,
2.54380826092923));
#6407=CARTESIAN_POINT('Ctrl Pts',(-25.0603014453932,-0.502555351656382,
2.54000886254707));
#6408=CARTESIAN_POINT('Ctrl Pts',(-25.0771344181921,-0.530461627229323,
2.53217843551044));
#6409=CARTESIAN_POINT('Ctrl Pts',(-25.0859109306211,-0.544239963564881,
2.52814434334757));
#6410=CARTESIAN_POINT('Ctrl Pts',(-25.1041597996001,-0.571392063284267,
2.51987677295435));
#6411=CARTESIAN_POINT('Ctrl Pts',(-25.1135652356457,-0.584667955785163,
2.51567359591458));
#6412=CARTESIAN_POINT('Ctrl Pts',(-25.1329503931644,-0.610672109363501,
2.50714732573442));
#6413=CARTESIAN_POINT('Ctrl Pts',(-25.1429262744659,-0.623394578020972,
2.50282595067223));
#6414=CARTESIAN_POINT('Ctrl Pts',(-25.1736949347874,-0.660743188336079,
2.48973044146157));
#6415=CARTESIAN_POINT('Ctrl Pts',(-25.1953265696652,-0.684552408790031,
2.48082441641631));
#6416=CARTESIAN_POINT('Ctrl Pts',(-25.2294621790932,-0.718669526189459,
2.46737442476458));
#6417=CARTESIAN_POINT('Ctrl Pts',(-25.2411226141971,-0.729775262858415,
2.46287588038062));
#6418=CARTESIAN_POINT('Ctrl Pts',(-25.2650163395357,-0.751453108570394,
2.45387816269178));
#6419=CARTESIAN_POINT('Ctrl Pts',(-25.2772554632753,-0.762029504500183,
2.44937698167527));
#6420=CARTESIAN_POINT('Ctrl Pts',(-25.3022971286316,-0.782626892006877,
2.44041267983556));
#6421=CARTESIAN_POINT('Ctrl Pts',(-25.315157197433,-0.792689421921387,2.43593042229927));
#6422=CARTESIAN_POINT('Ctrl Pts',(-25.341232755504,-0.812083164942917,2.42711283865451));
#6423=CARTESIAN_POINT('Ctrl Pts',(-25.3544672859955,-0.821434074532997,
2.42276972387511));
#6424=CARTESIAN_POINT('Ctrl Pts',(-25.3813264071519,-0.839452527788181,
2.41424554238549));
#6425=CARTESIAN_POINT('Ctrl Pts',(-25.3949513697869,-0.848120793930842,
2.41006421940509));
#6426=CARTESIAN_POINT('Ctrl Pts',(-25.4225940554056,-0.864782458141236,
2.40189271204072));
#6427=CARTESIAN_POINT('Ctrl Pts',(-25.4366117834694,-0.872775835903153,
2.39790249830954));
#6428=CARTESIAN_POINT('Ctrl Pts',(-25.479261734589,-0.895745723912417,2.386263986526));
#6429=CARTESIAN_POINT('Ctrl Pts',(-25.5084958123966,-0.909716954879009,
2.3789457429218));
#6430=CARTESIAN_POINT('Ctrl Pts',(-25.5535776615725,-0.928607298291761,
2.36882679203486));
#6431=CARTESIAN_POINT('Ctrl Pts',(-25.5688253899689,-0.934563660377399,
2.36559439343673));
#6432=CARTESIAN_POINT('Ctrl Pts',(-25.5920023693806,-0.942963605388763,
2.36098892152975));
#6433=CARTESIAN_POINT('Ctrl Pts',(-25.5997879839068,-0.94567716643989,2.35949277008249));
#6434=CARTESIAN_POINT('Ctrl Pts',(-25.6154612044865,-0.950922793268216,
2.35658631440842));
#6435=CARTESIAN_POINT('Ctrl Pts',(-25.6233613960042,-0.953458374961467,
2.35517402568802));
#6436=CARTESIAN_POINT('Ctrl Pts',(-25.6470876486476,-0.960748669979318,
2.35109499689056));
#6437=CARTESIAN_POINT('Ctrl Pts',(-25.6629694924038,-0.965199959788432,
2.34857921219019));
#6438=CARTESIAN_POINT('Ctrl Pts',(-25.6948784413748,-0.973301096108641,
2.34396841563555));
#6439=CARTESIAN_POINT('Ctrl Pts',(-25.710902645268,-0.976950283068506,2.34187376666204));
#6440=CARTESIAN_POINT('Ctrl Pts',(-25.7591844222772,-0.986703415822536,
2.33624500537071));
#6441=CARTESIAN_POINT('Ctrl Pts',(-25.791650783833,-0.991615665333941,2.33336629059962));
#6442=CARTESIAN_POINT('Ctrl Pts',(-25.8407756179032,-0.996582697577232,
2.3304458498952));
#6443=CARTESIAN_POINT('Ctrl Pts',(-25.8572215351598,-0.997837487879419,
2.329705241771));
#6444=CARTESIAN_POINT('Ctrl Pts',(-25.8902578614934,-0.999533165226665,
2.32870354106611));
#6445=CARTESIAN_POINT('Ctrl Pts',(-25.9068578724972,-0.999973524878361,
2.32844279123645));
#6446=CARTESIAN_POINT('Ctrl Pts',(-25.940167362761,-1.0000242628141,2.32841276730314));
#6447=CARTESIAN_POINT('Ctrl Pts',(-25.9569704588412,-0.999628762374181,
2.32864698234144));
#6448=CARTESIAN_POINT('Ctrl Pts',(-25.9903233075244,-0.998003316619995,
2.32960735397222));
#6449=CARTESIAN_POINT('Ctrl Pts',(-26.0069064582144,-0.99677776727011,2.33033089082929));
#6450=CARTESIAN_POINT('Ctrl Pts',(-26.0398870987565,-0.993516757651968,
2.33224874868744));
#6451=CARTESIAN_POINT('Ctrl Pts',(-26.0562852280577,-0.991481744891029,
2.33344279183591));
#6452=CARTESIAN_POINT('Ctrl Pts',(-26.0889006503167,-0.986614637292695,
2.33628332558741));
#6453=CARTESIAN_POINT('Ctrl Pts',(-26.1051179364934,-0.983782507538745,
2.33792982096873));
#6454=CARTESIAN_POINT('Ctrl Pts',(-26.1535021710044,-0.974099057442964,
2.34352095101131));
#6455=CARTESIAN_POINT('Ctrl Pts',(-26.1854056292135,-0.966060458399386,
2.3481189625644));
#6456=CARTESIAN_POINT('Ctrl Pts',(-26.2248342916283,-0.954027413144459,
2.35485651240159));
#6457=CARTESIAN_POINT('Ctrl Pts',(-26.2327013987641,-0.951518784920255,
2.35625480890824));
#6458=CARTESIAN_POINT('Ctrl Pts',(-26.2483827345867,-0.946304393522068,
2.35914625498642));
#6459=CARTESIAN_POINT('Ctrl Pts',(-26.2562117486977,-0.94359270504545,2.36064260344912));
#6460=CARTESIAN_POINT('Ctrl Pts',(-26.2795250530157,-0.935192248164096,
2.3652521259866));
#6461=CARTESIAN_POINT('Ctrl Pts',(-26.2948382163531,-0.929240340102424,
2.36848474521895));
#6462=CARTESIAN_POINT('Ctrl Pts',(-26.325052120344,-0.916638547977859,2.37524073173657));
#6463=CARTESIAN_POINT('Ctrl Pts',(-26.3399478665267,-0.90999062203962,2.37876303600403));
#6464=CARTESIAN_POINT('Ctrl Pts',(-26.3693289871196,-0.896011395896082,
2.38606310676974));
#6465=CARTESIAN_POINT('Ctrl Pts',(-26.3838143473607,-0.888680076643438,
2.38984089454833));
#6466=CARTESIAN_POINT('Ctrl Pts',(-26.4123832482896,-0.873338683184522,
2.3976202355067));
#6467=CARTESIAN_POINT('Ctrl Pts',(-26.4264667819849,-0.865328603021505,
2.40162180862374));
#6468=CARTESIAN_POINT('Ctrl Pts',(-26.4542373250601,-0.848628527049356,
2.40981807440537));
#6469=CARTESIAN_POINT('Ctrl Pts',(-26.4679244024272,-0.839938487173806,
2.41401280980997));
#6470=CARTESIAN_POINT('Ctrl Pts',(-26.4949038618746,-0.821871746929689,
2.42256536268358));
#6471=CARTESIAN_POINT('Ctrl Pts',(-26.5081993038235,-0.812492795486007,
2.42692421965941));
#6472=CARTESIAN_POINT('Ctrl Pts',(-26.5343829028199,-0.793043775382972,
2.43577160005359));
#6473=CARTESIAN_POINT('Ctrl Pts',(-26.5471738340693,-0.7830463803841,2.44022699893486));
#6474=CARTESIAN_POINT('Ctrl Pts',(-26.5721868510483,-0.762503182417991,
2.4491738057699));
#6475=CARTESIAN_POINT('Ctrl Pts',(-26.5844064334615,-0.751959204775381,
2.45366439347184));
#6476=CARTESIAN_POINT('Ctrl Pts',(-26.6082843084103,-0.730330096168273,
2.46264911716722));
#6477=CARTESIAN_POINT('Ctrl Pts',(-26.6199425628188,-0.719244941847823,
2.46714330180598));
#6478=CARTESIAN_POINT('Ctrl Pts',(-26.6540867150583,-0.685176365586002,
2.48058665935111));
#6479=CARTESIAN_POINT('Ctrl Pts',(-26.6757462073237,-0.661378975879618,
2.48949782346477));
#6480=CARTESIAN_POINT('Ctrl Pts',(-26.706573146655,-0.624022706324938,2.50261037529357));
#6481=CARTESIAN_POINT('Ctrl Pts',(-26.7165759724886,-0.611286384102542,
2.50694112711597));
#6482=CARTESIAN_POINT('Ctrl Pts',(-26.7311533876529,-0.591762476370502,
2.51334967146033));
#6483=CARTESIAN_POINT('Ctrl Pts',(-26.7359451890069,-0.585178854079478,
2.51547299658858));
#6484=CARTESIAN_POINT('Ctrl Pts',(-26.7453814833122,-0.571874856074331,
2.51968511284943));
#6485=CARTESIAN_POINT('Ctrl Pts',(-26.7500351366602,-0.565140645160058,
2.52177806865428));
#6486=CARTESIAN_POINT('Ctrl Pts',(-26.7637222516845,-0.544804309725444,
2.52797665659196));
#6487=CARTESIAN_POINT('Ctrl Pts',(-26.7724803391795,-0.531075645530332,
2.53200078580808));
#6488=CARTESIAN_POINT('Ctrl Pts',(-26.7892946991393,-0.503248393728809,
2.53981950802605));
#6489=CARTESIAN_POINT('Ctrl Pts',(-26.7973477617837,-0.489154779345306,
2.54361267297453));
#6490=CARTESIAN_POINT('Ctrl Pts',(-26.8204545728125,-0.446333368005571,
2.55461135090607));
#6491=CARTESIAN_POINT('Ctrl Pts',(-26.834458477791,-0.417066232433276,2.56143651401679));
#6492=CARTESIAN_POINT('Ctrl Pts',(-26.8596488370896,-0.357057925052845,
2.57389950485307));
#6493=CARTESIAN_POINT('Ctrl Pts',(-26.8708365853539,-0.326307436876508,
2.57953848796632));
#6494=CARTESIAN_POINT('Ctrl Pts',(-26.8854203844307,-0.279045599412756,
2.58696737317913));
#6495=CARTESIAN_POINT('Ctrl Pts',(-26.8899176876621,-0.263080836121057,
2.58927356668171));
#6496=CARTESIAN_POINT('Ctrl Pts',(-26.8981471118759,-0.230786385702436,
2.59351339304777));
#6497=CARTESIAN_POINT('Ctrl Pts',(-26.901854302142,-0.214553907874612,2.59543412523402));
#6498=CARTESIAN_POINT('Ctrl Pts',(-26.9084607843892,-0.181886203010055,
2.59886924230702));
#6499=CARTESIAN_POINT('Ctrl Pts',(-26.9113574905324,-0.165464138876776,
2.6003822869898));
#6500=CARTESIAN_POINT('Ctrl Pts',(-26.9163383589761,-0.132393422445163,
2.60299055921658));
#6501=CARTESIAN_POINT('Ctrl Pts',(-26.9184105531932,-0.1158177180384,2.60407951595309));
#6502=CARTESIAN_POINT('Ctrl Pts',(-26.9233593618272,-0.0661859402484176,
2.60668400705037));
#6503=CARTESIAN_POINT('Ctrl Pts',(-26.9249972922528,-0.0331164849794928,
2.60755116529974));
#6504=CARTESIAN_POINT('Ctrl Pts',(-26.9250013487368,0.016434104258675,2.60755332849863));
#6505=CARTESIAN_POINT('Ctrl Pts',(-26.924593771391,0.0329435135702283,2.60733786318112));
#6506=CARTESIAN_POINT('Ctrl Pts',(-26.9229598784543,0.0659474161951004,
2.60647540292584));
#6507=CARTESIAN_POINT('Ctrl Pts',(-26.9217335860717,0.0824419098590674,
2.60582840846348));
#6508=CARTESIAN_POINT('Ctrl Pts',(-26.9184554239328,0.115415878608658,2.60410310617677));
#6509=CARTESIAN_POINT('Ctrl Pts',(-26.9164025400161,0.131898834522029,2.60302426431673));
#6510=CARTESIAN_POINT('Ctrl Pts',(-26.9114621352338,0.164835602978561,2.60043699179505));
#6511=CARTESIAN_POINT('Ctrl Pts',(-26.9085613270678,0.181339949722123,2.59892168747799));
#6512=CARTESIAN_POINT('Ctrl Pts',(-26.9019944221297,0.213908268855232,2.59550682162746));
#6513=CARTESIAN_POINT('Ctrl Pts',(-26.8983181557807,0.230051496944321,2.59360192011072));
#6514=CARTESIAN_POINT('Ctrl Pts',(-26.8902038146127,0.262018183387905,2.58942059752269));
#6515=CARTESIAN_POINT('Ctrl Pts',(-26.8857646886985,0.27784935865575,2.58714361859994));
#6516=CARTESIAN_POINT('Ctrl Pts',(-26.8713188216695,0.324895801813618,2.57978251945633));
#6517=CARTESIAN_POINT('Ctrl Pts',(-26.8601834035885,0.355670011650616,2.5741669021953));
#6518=CARTESIAN_POINT('Ctrl Pts',(-26.8412500664846,0.400941255234932,2.56479529641426));
#6519=CARTESIAN_POINT('Ctrl Pts',(-26.8345604461981,0.415894450482944,2.56151035689196));
#6520=CARTESIAN_POINT('Ctrl Pts',(-26.8239684235737,0.438090391025238,2.55636178150267));
#6521=CARTESIAN_POINT('Ctrl Pts',(-26.8203410661095,0.44545683266115,2.55460695983525));
#6522=CARTESIAN_POINT('Ctrl Pts',(-26.8128999456829,0.460110113434811,2.55102621846157));
#6523=CARTESIAN_POINT('Ctrl Pts',(-26.8090809400854,0.467406099051343,2.54919783195029));
#6524=CARTESIAN_POINT('Ctrl Pts',(-26.7973956024953,0.489075501379372,2.54363495988492));
#6525=CARTESIAN_POINT('Ctrl Pts',(-26.7892904087949,0.503256366320305,2.53981745826164));
#6526=CARTESIAN_POINT('Ctrl Pts',(-26.7724556899274,0.531115565582863,2.53198937867128));
#6527=CARTESIAN_POINT('Ctrl Pts',(-26.7637274203706,0.544791910987857,2.5279793571639));
#6528=CARTESIAN_POINT('Ctrl Pts',(-26.7366217266702,0.58507967901888,2.51570272134659));
#6529=CARTESIAN_POINT('Ctrl Pts',(-26.7173257403855,0.61095146719629,2.50718915145592));
#6530=CARTESIAN_POINT('Ctrl Pts',(-26.6865421652591,0.648316199104956,2.49408756309351));
#6531=CARTESIAN_POINT('Ctrl Pts',(-26.6759737885839,0.660530164014685,2.48966507904171));
#6532=CARTESIAN_POINT('Ctrl Pts',(-26.6542143618837,0.684476541997761,2.48073725881267));
#6533=CARTESIAN_POINT('Ctrl Pts',(-26.6430275831957,0.696204572944761,2.47623358134869));
#6534=CARTESIAN_POINT('Ctrl Pts',(-26.625757459411,0.71344606171305,2.46943219638785));
#6535=CARTESIAN_POINT('Ctrl Pts',(-26.619921440287,0.719131601096507,2.46715852858783));
#6536=CARTESIAN_POINT('Ctrl Pts',(-26.6081492806517,0.730323844266242,2.4626246472445));
#6537=CARTESIAN_POINT('Ctrl Pts',(-26.6022023493564,0.735841448132364,2.46036016392892));
#6538=CARTESIAN_POINT('Ctrl Pts',(-26.5841990801845,0.752142596351644,2.4535872758574));
#6539=CARTESIAN_POINT('Ctrl Pts',(-26.5719637153137,0.762691293347724,2.44909283533733));
#6540=CARTESIAN_POINT('Ctrl Pts',(-26.5345859666616,0.79337500010439,2.43572683396234));
#6541=CARTESIAN_POINT('Ctrl Pts',(-26.5087543078564,0.812569281368953,2.42696429363966));
#6542=CARTESIAN_POINT('Ctrl Pts',(-26.4686216279805,0.839484914822931,2.41422981442002));
#6543=CARTESIAN_POINT('Ctrl Pts',(-26.4550122677061,0.848144060795981,2.41005301554826));
#6544=CARTESIAN_POINT('Ctrl Pts',(-26.4273198206187,0.864833014186361,2.4018677094334));
#6545=CARTESIAN_POINT('Ctrl Pts',(-26.4132367723247,0.872862861793055,2.39785915569383));
#6546=CARTESIAN_POINT('Ctrl Pts',(-26.3845827730249,0.888283954759512,2.39004399122574));
#6547=CARTESIAN_POINT('Ctrl Pts',(-26.3700175910458,0.895672296665482,2.38623887159213));
#6548=CARTESIAN_POINT('Ctrl Pts',(-26.3477725177819,0.906273162875091,2.38070494715483));
#6549=CARTESIAN_POINT('Ctrl Pts',(-26.3402926727503,0.909725000544916,2.37888997766035));
#6550=CARTESIAN_POINT('Ctrl Pts',(-26.3252947580114,0.91642317054735,2.37534522135332));
#6551=CARTESIAN_POINT('Ctrl Pts',(-26.3177609641362,0.919677618978277,2.37361127867655));
#6552=CARTESIAN_POINT('Ctrl Pts',(-26.279960326246,0.935453358182173,2.36515451304933));
#6553=CARTESIAN_POINT('Ctrl Pts',(-26.2492308175849,0.946541064909445,2.35904578187965));
#6554=CARTESIAN_POINT('Ctrl Pts',(-26.1868089918217,0.965671617244593,2.3483390844543));
#6555=CARTESIAN_POINT('Ctrl Pts',(-26.1551127594127,0.973718288717797,2.3437391769445));
#6556=CARTESIAN_POINT('Ctrl Pts',(-26.1068144462703,0.983469972772359,2.33811102541253));
#6557=CARTESIAN_POINT('Ctrl Pts',(-26.090589178399,0.986333510705604,2.3364469269674));
#6558=CARTESIAN_POINT('Ctrl Pts',(-26.0578800212193,0.991270124222091,2.33356672209885));
#6559=CARTESIAN_POINT('Ctrl Pts',(-26.0413989600866,0.993342685095568,2.33235094950619));
#6560=CARTESIAN_POINT('Ctrl Pts',(-26.016468400417,0.995843155056375,2.33088062949276));
#6561=CARTESIAN_POINT('Ctrl Pts',(-26.0081137802036,0.996575200948386,2.33044941555122));
#6562=CARTESIAN_POINT('Ctrl Pts',(-25.9914406456729,0.997825328960478,2.32971229361947));
#6563=CARTESIAN_POINT('Ctrl Pts',(-25.9831090698346,0.998345104091185,2.32940539355606));
#6564=CARTESIAN_POINT('Ctrl Pts',(-25.9581619918789,0.999588413090816,2.32867085845434));
#6565=CARTESIAN_POINT('Ctrl Pts',(-25.9415535789236,1.00000042873077,2.3284268504534));
#6566=CARTESIAN_POINT('Ctrl Pts',(-25.8918801116583,0.999999142511444,2.32842767334732));
#6567=CARTESIAN_POINT('Ctrl Pts',(-25.8588976369251,0.998358102087351,2.32940162628822));
#6568=CARTESIAN_POINT('Ctrl Pts',(-25.809655452566,0.993462469088689,2.33228059590287));
#6569=CARTESIAN_POINT('Ctrl Pts',(-25.7932780679245,0.991424398396008,2.33347638591532));
#6570=CARTESIAN_POINT('Ctrl Pts',(-25.7605967018549,0.986531578876194,2.33633167075591));
#6571=CARTESIAN_POINT('Ctrl Pts',(-25.744287250752,0.983675445441529,2.3379919778889));
#6572=CARTESIAN_POINT('Ctrl Pts',(-25.7198948761487,0.978775245710681,2.34082078278938));
#6573=CARTESIAN_POINT('Ctrl Pts',(-25.7117693154796,0.97703729202741,2.34182114664376));
#6574=CARTESIAN_POINT('Ctrl Pts',(-25.6955363910876,0.973352864470024,2.34393407887515));
#6575=CARTESIAN_POINT('Ctrl Pts',(-25.6874340994824,0.971407041360756,2.34504624803508));
#6576=CARTESIAN_POINT('Ctrl Pts',(-25.6632984183101,0.965291239666668,2.3485275986422));
#6577=CARTESIAN_POINT('Ctrl Pts',(-25.6473893995262,0.960834612092796,2.35104651772394));
#6578=CARTESIAN_POINT('Ctrl Pts',(-25.6159251530686,0.951180080790835,2.35644914953997));
#6579=CARTESIAN_POINT('Ctrl Pts',(-25.6003693864663,0.945982332371016,2.35933277792001));
#6580=CARTESIAN_POINT('Ctrl Pts',(-25.5696010487147,0.934857849827407,2.36543410266168));
#6581=CARTESIAN_POINT('Ctrl Pts',(-25.554388497757,0.928931075544407,2.36865182569908));
#6582=CARTESIAN_POINT('Ctrl Pts',(-25.5092553225566,0.910065915709691,2.378761754307));
#6583=CARTESIAN_POINT('Ctrl Pts',(-25.4798364380125,0.896042727572782,2.3861116959914));
#6584=CARTESIAN_POINT('Ctrl Pts',(-25.4438909156586,0.876699211680765,2.39591502278523));
#6585=CARTESIAN_POINT('Ctrl Pts',(-25.4367414461902,0.872737300160877,2.39790741951298));
#6586=CARTESIAN_POINT('Ctrl Pts',(-25.4225293356803,0.864633016249678,2.40194902287731));
#6587=CARTESIAN_POINT('Ctrl Pts',(-25.4154580969326,0.860484766397168,2.40400099723935));
#6588=CARTESIAN_POINT('Ctrl Pts',(-25.3944657161042,0.847820800232131,2.41021024122678));
#6589=CARTESIAN_POINT('Ctrl Pts',(-25.380746070164,0.839077244133138,2.41442548123448));
#6590=CARTESIAN_POINT('Ctrl Pts',(-25.3538260232817,0.820989195886628,2.42297767676368));
#6591=CARTESIAN_POINT('Ctrl Pts',(-25.3406279393829,0.811646297981065,2.42731389565943));
#6592=CARTESIAN_POINT('Ctrl Pts',(-25.3147430597672,0.792367900936231,2.43607407349852));
#6593=CARTESIAN_POINT('Ctrl Pts',(-25.3020562810124,0.782432389835529,2.44049806007427));
#6594=CARTESIAN_POINT('Ctrl Pts',(-25.2771860341754,0.761968758341592,2.4494026816381));
#6595=CARTESIAN_POINT('Ctrl Pts',(-25.2650025732109,0.751440637442868,2.45388334271684));
#6596=CARTESIAN_POINT('Ctrl Pts',(-25.2411353303519,0.729786781206718,2.46287109582098));
#6597=CARTESIAN_POINT('Ctrl Pts',(-25.2294515461917,0.718661056693567,2.46737821378511));
#6598=CARTESIAN_POINT('Ctrl Pts',(-25.2065843288473,0.695801899103863,2.47638907712378));
#6599=CARTESIAN_POINT('Ctrl Pts',(-25.1954014188971,0.684068711345197,2.48089267439045));
#6600=CARTESIAN_POINT('Ctrl Pts',(-25.1790045373378,0.666000870018046,2.48762367211154));
#6601=CARTESIAN_POINT('Ctrl Pts',(-25.1735960376354,0.659892776183967,2.48986579326023));
#6602=CARTESIAN_POINT('Ctrl Pts',(-25.1629494208789,0.647568638488018,2.49431990834339));
#6603=CARTESIAN_POINT('Ctrl Pts',(-25.1577105174054,0.641352897528938,2.49653204883515));
#6604=CARTESIAN_POINT('Ctrl Pts',(-25.1319358378313,0.610000274169434,2.50751029184406));
#6605=CARTESIAN_POINT('Ctrl Pts',(-25.1126431635002,0.584053957250259,2.51603030353834));
#6606=CARTESIAN_POINT('Ctrl Pts',(-25.0766559633797,0.53042915613372,2.53234045288691));
#6607=CARTESIAN_POINT('Ctrl Pts',(-25.0599598863832,0.502751233364297,2.54013165293879));
#6608=CARTESIAN_POINT('Ctrl Pts',(-25.0368787132278,0.459895387665409,2.55112212486568));
#6609=CARTESIAN_POINT('Ctrl Pts',(-25.0295127265205,0.445386602515356,2.55466961647924));
#6610=CARTESIAN_POINT('Ctrl Pts',(-25.015447538885,0.415909836891662,2.56150652151535));
#6611=CARTESIAN_POINT('Ctrl Pts',(-25.0087479847154,0.400940313195683,2.56479614450175));
#6612=CARTESIAN_POINT('Ctrl Pts',(-24.9992124578344,0.378134446441368,2.56951620636084));
#6613=CARTESIAN_POINT('Ctrl Pts',(-24.9961153890925,0.370461653972984,2.57105596109368));
#6614=CARTESIAN_POINT('Ctrl Pts',(-24.9901146400105,0.35504609621479,2.57405082283814));
#6615=CARTESIAN_POINT('Ctrl Pts',(-24.9872162178828,0.347318031889454,2.57550327285404));
#6616=CARTESIAN_POINT('Ctrl Pts',(-24.978823527118,0.324069285671265,2.57972387330156));
#6617=CARTESIAN_POINT('Ctrl Pts',(-24.9736218334904,0.308462402151712,2.58236010535198));
#6618=CARTESIAN_POINT('Ctrl Pts',(-24.9640099750406,0.277069749192375,2.58725894187429));
#6619=CARTESIAN_POINT('Ctrl Pts',(-24.9595973255169,0.261278097086917,2.58952279476209));
#6620=CARTESIAN_POINT('Ctrl Pts',(-24.9515543557535,0.229504132582814,2.59366790173025));
#6621=CARTESIAN_POINT('Ctrl Pts',(-24.9479240403419,0.21352182008315,2.59554916744327));
#6622=CARTESIAN_POINT('Ctrl Pts',(-24.941447441202,0.181365268356563,2.59891718319404));
#6623=CARTESIAN_POINT('Ctrl Pts',(-24.9386011499407,0.165191031604556,2.60040394522677));
#6624=CARTESIAN_POINT('Ctrl Pts',(-24.9337002237304,0.132648091777223,2.60297035508353));
#6625=CARTESIAN_POINT('Ctrl Pts',(-24.93164556828,0.116279393924669,2.60405001587272));
#6626=CARTESIAN_POINT('Ctrl Pts',(-24.928341708171,0.0833436511207344,2.60578872210515));
#6627=CARTESIAN_POINT('Ctrl Pts',(-24.9270927815557,0.0667757724171855,
2.60644761593105));
#6628=CARTESIAN_POINT('Ctrl Pts',(-24.9258378814317,0.041773714006671,2.60711000800063));
#6629=CARTESIAN_POINT('Ctrl Pts',(-24.9255229363957,0.0334016706388515,
2.60727635262696));
#6630=CARTESIAN_POINT('Ctrl Pts',(-24.9251040599288,0.0166741935422472,
2.60749761997639));
#6631=CARTESIAN_POINT('Ctrl Pts',(-24.9249998216784,0.00832709294464485,
2.6075527040951));
#6632=CARTESIAN_POINT('Ctrl Pts',(-24.925,1.55854062294791E-16,2.60755260924175));
#6633=CARTESIAN_POINT('',(-27.0987792489536,-0.00011176064453429,2.99999999791826));
#6634=CARTESIAN_POINT('',(-24.7512207470268,-1.35620146123698E-16,3.));
#6635=CARTESIAN_POINT('Ctrl Pts',(-27.0987792489536,-0.000111760644534305,
2.99999999791826));
#6636=CARTESIAN_POINT('Ctrl Pts',(-27.098788175703,0.125293846590081,3.00000466972209));
#6637=CARTESIAN_POINT('Ctrl Pts',(-27.0836572608919,0.249887612487841,2.9920480612095));
#6638=CARTESIAN_POINT('Ctrl Pts',(-27.0242841101371,0.48924794879498,2.96225146824175));
#6639=CARTESIAN_POINT('Ctrl Pts',(-26.9807678619007,0.603149705374038,2.94076784698434));
#6640=CARTESIAN_POINT('Ctrl Pts',(-26.8427192011934,0.860536585807651,2.87814965124371));
#6641=CARTESIAN_POINT('Ctrl Pts',(-26.7376907200816,0.989566183851768,2.83419679721349));
#6642=CARTESIAN_POINT('Ctrl Pts',(-26.5155467319979,1.17588715226968,2.76143949975893));
#6643=CARTESIAN_POINT('Ctrl Pts',(-26.4004065512224,1.24404280001839,2.73036038773098));
#6644=CARTESIAN_POINT('Ctrl Pts',(-26.1626806024216,1.32927584783701,2.68979319984401));
#6645=CARTESIAN_POINT('Ctrl Pts',(-26.045246827223,1.35044153732405,2.67886312720281));
#6646=CARTESIAN_POINT('Ctrl Pts',(-25.8046235970333,1.35043417397338,2.67886683912841));
#6647=CARTESIAN_POINT('Ctrl Pts',(-25.6870707985615,1.32923939483604,2.68981328055148));
#6648=CARTESIAN_POINT('Ctrl Pts',(-25.449853763149,1.24407674422564,2.73034115324469));
#6649=CARTESIAN_POINT('Ctrl Pts',(-25.3353287651276,1.17639337787472,2.76120614485189));
#6650=CARTESIAN_POINT('Ctrl Pts',(-25.1094606312558,0.987455834851943,2.83506483214577));
#6651=CARTESIAN_POINT('Ctrl Pts',(-25.0061794065546,0.857630793528194,2.87869860737062));
#6652=CARTESIAN_POINT('Ctrl Pts',(-24.8702787932864,0.605712510755168,2.94025713869639));
#6653=CARTESIAN_POINT('Ctrl Pts',(-24.8263223973941,0.491220877838436,2.96195070021859));
#6654=CARTESIAN_POINT('Ctrl Pts',(-24.7664326588165,0.250724694262543,2.99199929730303));
#6655=CARTESIAN_POINT('Ctrl Pts',(-24.7512189476652,0.125688720919145,3.));
#6656=CARTESIAN_POINT('Ctrl Pts',(-24.7512207470268,-1.77808824465813E-16,
3.));
#6657=CARTESIAN_POINT('',(-26.9249999965755,-8.27588207139558E-5,2.60755260743233));
#6658=CARTESIAN_POINT('',(-27.0987792489536,-0.00011176064453429,2.99999999791826));
#6659=CARTESIAN_POINT('',(-26.925,-1.22464679914735E-16,2.60755336253159));
#6660=CARTESIAN_POINT('Ctrl Pts',(-26.9249999965755,-8.27588207141801E-5,
2.60755260743234));
#6661=CARTESIAN_POINT('Ctrl Pts',(-26.9249999988585,-5.51724988970155E-5,
2.60755260869231));
#6662=CARTESIAN_POINT('Ctrl Pts',(-26.925,-2.75862252988456E-5,2.60755260934744));
#6663=CARTESIAN_POINT('Ctrl Pts',(-26.925,-1.18762492463923E-16,2.60755260939777));
#6664=CARTESIAN_POINT('',(-24.925,7.79270311473956E-17,2.60755260924175));
#6665=CARTESIAN_POINT('Ctrl Pts',(-26.925,-1.18762492463923E-16,2.60755260939777));
#6666=CARTESIAN_POINT('Ctrl Pts',(-26.925,0.056804854575246,2.60755271302727));
#6667=CARTESIAN_POINT('Ctrl Pts',(-26.9201545072349,0.11340491023323,2.60497728285419));
#6668=CARTESIAN_POINT('Ctrl Pts',(-26.9010104955459,0.22498623920327,2.5949812948901));
#6669=CARTESIAN_POINT('Ctrl Pts',(-26.8867435237432,0.279664869028097,2.58757303140779));
#6670=CARTESIAN_POINT('Ctrl Pts',(-26.8304379456036,0.439261093144634,2.55919607531663));
#6671=CARTESIAN_POINT('Ctrl Pts',(-26.7755419497675,0.537393100961416,2.5323069913651));
#6672=CARTESIAN_POINT('Ctrl Pts',(-26.6644533472358,0.676591305065292,2.48451442941931));
#6673=CARTESIAN_POINT('Ctrl Pts',(-26.6171007671406,0.72494248878711,2.46539574358495));
#6674=CARTESIAN_POINT('Ctrl Pts',(-26.4737133682738,0.844473887402666,2.41369606443502));
#6675=CARTESIAN_POINT('Ctrl Pts',(-26.36820386171,0.904656958254169,2.38211334429286));
#6676=CARTESIAN_POINT('Ctrl Pts',(-26.1484453864065,0.980999063110147,2.34001084161921));
#6677=CARTESIAN_POINT('Ctrl Pts',(-26.0378922085563,1.00000218800714,2.32842180399996));
#6678=CARTESIAN_POINT('Ctrl Pts',(-25.8119011916325,0.999997808364593,2.32843245470472));
#6679=CARTESIAN_POINT('Ctrl Pts',(-25.7011902899078,0.980940359915184,2.3400492095282));
#6680=CARTESIAN_POINT('Ctrl Pts',(-25.4813838789149,0.904439026472466,2.38222657916133));
#6681=CARTESIAN_POINT('Ctrl Pts',(-25.3760142250183,0.844278486742472,2.41378709535218));
#6682=CARTESIAN_POINT('Ctrl Pts',(-25.1812462928254,0.681847452255209,2.48402790420268));
#6683=CARTESIAN_POINT('Ctrl Pts',(-25.095560456034,0.575048470588331,2.52290226852294));
#6684=CARTESIAN_POINT('Ctrl Pts',(-24.998457233114,0.384117255242701,2.56961701508285));
#6685=CARTESIAN_POINT('Ctrl Pts',(-24.9711794271723,0.310565523100897,2.58353335930288));
#6686=CARTESIAN_POINT('Ctrl Pts',(-24.9343517093779,0.15745257163897,2.60255728285402));
#6687=CARTESIAN_POINT('Ctrl Pts',(-24.925,0.0790612261660938,2.60754968635441));
#6688=CARTESIAN_POINT('Ctrl Pts',(-24.925,1.53956708492938E-16,2.60755260924175));
#6689=CARTESIAN_POINT('',(-24.7512207470268,-1.35620146123698E-16,3.));
#6690=CARTESIAN_POINT('Origin',(-28.425,0.,0.));
#6691=CARTESIAN_POINT('',(-21.125,-2.82842712474618,1.00000000000001));
#6692=CARTESIAN_POINT('',(-21.125,-2.82842712474618,-1.00000000000001));
#6693=CARTESIAN_POINT('Origin',(-21.125,1.33651518465759E-15,0.));
#6694=CARTESIAN_POINT('',(-28.425,-2.82842712474619,-1.00000000000001));
#6695=CARTESIAN_POINT('',(-28.425,-2.82842712474619,-1.00000000000001));
#6696=CARTESIAN_POINT('',(-28.425,2.82842712474619,-1.00000000000001));
#6697=CARTESIAN_POINT('Origin',(-28.425,1.00559551819496E-31,0.));
#6698=CARTESIAN_POINT('',(-21.125,2.82842712474619,-1.00000000000001));
#6699=CARTESIAN_POINT('',(-28.425,2.82842712474619,-1.00000000000001));
#6700=CARTESIAN_POINT('',(-21.125,3.,-3.67394039744206E-16));
#6701=CARTESIAN_POINT('Origin',(-21.125,1.33651518465759E-15,0.));
#6702=CARTESIAN_POINT('',(-20.325,3.,-3.67394039744206E-16));
#6703=CARTESIAN_POINT('',(-28.425,3.,-3.67394039744206E-16));
#6704=CARTESIAN_POINT('Origin',(-20.325,9.30296956444027E-16,0.));
#6705=CARTESIAN_POINT('',(-21.125,2.82842712474619,0.999999999999995));
#6706=CARTESIAN_POINT('Origin',(-21.125,1.33651518465759E-15,0.));
#6707=CARTESIAN_POINT('',(-28.425,2.82842712474619,1.00000000000001));
#6708=CARTESIAN_POINT('',(-28.425,2.82842712474619,1.00000000000001));
#6709=CARTESIAN_POINT('',(-28.425,-2.82842712474619,1.00000000000001));
#6710=CARTESIAN_POINT('Origin',(-28.425,1.00559551819496E-31,0.));
#6711=CARTESIAN_POINT('',(-28.425,-2.82842712474619,1.00000000000001));
#6712=CARTESIAN_POINT('Ctrl Pts',(-24.7512207470268,1.465751492483E-15,
-3.));
#6713=CARTESIAN_POINT('Ctrl Pts',(-24.7512225835704,0.128285957454602,-3.));
#6714=CARTESIAN_POINT('Ctrl Pts',(-24.7670495401009,0.25583672234664,-2.99166914509907));
#6715=CARTESIAN_POINT('Ctrl Pts',(-24.8294109793546,0.500872203914624,-2.96042265250318));
#6716=CARTESIAN_POINT('Ctrl Pts',(-24.8750650035884,0.617122189157838,-2.9379400782468));
#6717=CARTESIAN_POINT('Ctrl Pts',(-25.014086994418,0.868531543834054,-2.87533793314114));
#6718=CARTESIAN_POINT('Ctrl Pts',(-25.1178167867906,0.996326582468178,-2.83188528988297));
#6719=CARTESIAN_POINT('Ctrl Pts',(-25.343381297619,1.1815076728687,-2.75895840349069));
#6720=CARTESIAN_POINT('Ctrl Pts',(-25.4571148445719,1.24753580132896,-2.72873792314024));
#6721=CARTESIAN_POINT('Ctrl Pts',(-25.7218191299461,1.34070762403808,-2.68430500111959));
#6722=CARTESIAN_POINT('Ctrl Pts',(-25.8409376382471,1.35029210277812,-2.67893845828434));
#6723=CARTESIAN_POINT('Ctrl Pts',(-26.0070593989418,1.35058323368467,-2.67879169700489));
#6724=CARTESIAN_POINT('Ctrl Pts',(-26.1263048541123,1.34103185276652,-2.684134010337));
#6725=CARTESIAN_POINT('Ctrl Pts',(-26.391961880762,1.24815768478947,-2.72845580912919));
#6726=CARTESIAN_POINT('Ctrl Pts',(-26.5066389202574,1.18160031466836,-2.75893875380659));
#6727=CARTESIAN_POINT('Ctrl Pts',(-26.7321634254033,0.99620726980863,-2.83191131674452));
#6728=CARTESIAN_POINT('Ctrl Pts',(-26.8354958588566,0.868962163429233,-2.8751698727339));
#6729=CARTESIAN_POINT('Ctrl Pts',(-26.9742467036987,0.618608250844591,-2.93761533941595));
#6730=CARTESIAN_POINT('Ctrl Pts',(-27.0198972430111,0.502744502919277,-2.96008325572955));
#6731=CARTESIAN_POINT('Ctrl Pts',(-27.0826499193283,0.257871735999257,-2.99151091633777));
#6732=CARTESIAN_POINT('Ctrl Pts',(-27.0987700470889,0.129382268032874,-2.99999518213318));
#6733=CARTESIAN_POINT('Ctrl Pts',(-27.0987792489536,0.000111760644532495,
-2.99999999791826));
#6734=CARTESIAN_POINT('Ctrl Pts',(-24.7512207470268,-3.65455693999632E-16,
3.));
#6735=CARTESIAN_POINT('Ctrl Pts',(-24.7512225835705,-0.128285957454966,
3.));
#6736=CARTESIAN_POINT('Ctrl Pts',(-24.7670495401008,-0.255836722348032,
2.99166914509913));
#6737=CARTESIAN_POINT('Ctrl Pts',(-24.8294109793572,-0.500872203922864,
2.9604226525019));
#6738=CARTESIAN_POINT('Ctrl Pts',(-24.8750650035926,-0.617122189167466,
2.93794007824478));
#6739=CARTESIAN_POINT('Ctrl Pts',(-25.0140869944243,-0.868531543842818,
2.87533793313844));
#6740=CARTESIAN_POINT('Ctrl Pts',(-25.1178167867974,-0.996326582475323,
2.8318852898804));
#6741=CARTESIAN_POINT('Ctrl Pts',(-25.3433812976256,-1.18150767287279,2.75895840348889));
#6742=CARTESIAN_POINT('Ctrl Pts',(-25.4571148445771,-1.24753580133114,2.72873792313922));
#6743=CARTESIAN_POINT('Ctrl Pts',(-25.7218191299552,-1.34070762404087,2.68430500111824));
#6744=CARTESIAN_POINT('Ctrl Pts',(-25.8409376382588,-1.35029210277812,2.67893845828434));
#6745=CARTESIAN_POINT('Ctrl Pts',(-26.0070593989402,-1.35058323368466,2.67879169700489));
#6746=CARTESIAN_POINT('Ctrl Pts',(-26.12630485411,-1.34103185276689,2.6841340103368));
#6747=CARTESIAN_POINT('Ctrl Pts',(-26.3919618807593,-1.2481576847908,2.72845580912858));
#6748=CARTESIAN_POINT('Ctrl Pts',(-26.506638920255,-1.18160031466976,2.75893875380596));
#6749=CARTESIAN_POINT('Ctrl Pts',(-26.7321634253999,-0.996207269812109,
2.83191131674325));
#6750=CARTESIAN_POINT('Ctrl Pts',(-26.835495858853,-0.868962163433963,2.87516987273241));
#6751=CARTESIAN_POINT('Ctrl Pts',(-26.9742467036962,-0.618608250850395,
2.93761533941474));
#6752=CARTESIAN_POINT('Ctrl Pts',(-27.0198972430095,-0.502744502924232,
2.96008325572877));
#6753=CARTESIAN_POINT('Ctrl Pts',(-27.0826499193282,-0.257871736000858,
2.99151091633771));
#6754=CARTESIAN_POINT('Ctrl Pts',(-27.0987700470889,-0.129382268034096,
2.99999518213318));
#6755=CARTESIAN_POINT('Ctrl Pts',(-27.0987792489536,-0.000111760644534299,
2.99999999791826));
#6756=CARTESIAN_POINT('Origin',(-25.925,0.,-3.));
#6757=CARTESIAN_POINT('',(-26.925,-1.22464679914735E-16,-1.00000000000001));
#6758=CARTESIAN_POINT('',(-26.925,-1.22464679914735E-16,-3.));
#6759=CARTESIAN_POINT('Origin',(-25.925,0.,-1.00000000000001));
#6760=CARTESIAN_POINT('Ctrl Pts',(-26.9249999965755,8.27588207122151E-5,
-2.60755260743233));
#6761=CARTESIAN_POINT('Ctrl Pts',(-26.9249904249565,0.115739541719608,-2.60754732495302));
#6762=CARTESIAN_POINT('Ctrl Pts',(-26.9050186532092,0.229309368673701,-2.59676308014965));
#6763=CARTESIAN_POINT('Ctrl Pts',(-26.8283116849146,0.443793157962873,-2.55814777286124));
#6764=CARTESIAN_POINT('Ctrl Pts',(-26.7725502043353,0.542252124779991,-2.53089457930302));
#6765=CARTESIAN_POINT('Ctrl Pts',(-26.6216961833966,0.728812739977055,-2.46627281639632));
#6766=CARTESIAN_POINT('Ctrl Pts',(-26.5220865225859,0.812534660967263,-2.42818900421659));
#6767=CARTESIAN_POINT('Ctrl Pts',(-26.3104040242462,0.929588521928789,-2.36930439148383));
#6768=CARTESIAN_POINT('Ctrl Pts',(-26.2022893987898,0.967702137191157,-2.34728407052782));
#6769=CARTESIAN_POINT('Ctrl Pts',(-26.0338171724686,0.995597707881966,-2.33105492627662));
#6770=CARTESIAN_POINT('Ctrl Pts',(-25.9787262626432,1.00008101773999,-2.32837603269168));
#6771=CARTESIAN_POINT('Ctrl Pts',(-25.8686962905677,0.999917360916853,-2.32847915347898));
#6772=CARTESIAN_POINT('Ctrl Pts',(-25.8139981228262,0.995338596268691,-2.33120606433384));
#6773=CARTESIAN_POINT('Ctrl Pts',(-25.6457369572163,0.967153847373896,-2.34760035492249));
#6774=CARTESIAN_POINT('Ctrl Pts',(-25.537535323688,0.928753670996883,-2.36976707795452));
#6775=CARTESIAN_POINT('Ctrl Pts',(-25.3255406714156,0.810864803745833,-2.42897889523396));
#6776=CARTESIAN_POINT('Ctrl Pts',(-25.2257850797804,0.72648986790713,-2.46725895286466));
#6777=CARTESIAN_POINT('Ctrl Pts',(-25.0755270452445,0.539171378437474,-2.53180070351224));
#6778=CARTESIAN_POINT('Ctrl Pts',(-25.0202559439194,0.440786335108821,-2.55885563811918));
#6779=CARTESIAN_POINT('Ctrl Pts',(-24.9446246649158,0.227289219833161,-2.59695611074295));
#6780=CARTESIAN_POINT('Ctrl Pts',(-24.925,0.114639026798552,-2.60755684743726));
#6781=CARTESIAN_POINT('Ctrl Pts',(-24.925,2.65813431825893E-16,-2.60755260924174));
#6782=CARTESIAN_POINT('Origin',(-25.925,0.,-3.));
#6783=CARTESIAN_POINT('',(-26.925,-1.22464679914735E-16,1.));
#6784=CARTESIAN_POINT('Origin',(-25.925,0.,1.));
#6785=CARTESIAN_POINT('',(-26.925,-1.22464679914735E-16,-3.));
#6786=CARTESIAN_POINT('Ctrl Pts',(-26.9249999965755,-8.27588207141808E-5,
2.60755260743234));
#6787=CARTESIAN_POINT('Ctrl Pts',(-26.9249904249565,-0.115739541719426,
2.6075473249531));
#6788=CARTESIAN_POINT('Ctrl Pts',(-26.9050186532092,-0.229309368673756,
2.59676308014972));
#6789=CARTESIAN_POINT('Ctrl Pts',(-26.8283116849141,-0.443793157963809,
2.55814777286102));
#6790=CARTESIAN_POINT('Ctrl Pts',(-26.7725502043348,-0.542252124780864,
2.53089457930282));
#6791=CARTESIAN_POINT('Ctrl Pts',(-26.6216961833953,-0.728812739978349,
2.46627281639579));
#6792=CARTESIAN_POINT('Ctrl Pts',(-26.5220865225849,-0.81253466096794,2.42818900421627));
#6793=CARTESIAN_POINT('Ctrl Pts',(-26.3104040242456,-0.929588521929025,
2.36930439148371));
#6794=CARTESIAN_POINT('Ctrl Pts',(-26.202289398789,-0.967702137191383,2.3472840705277));
#6795=CARTESIAN_POINT('Ctrl Pts',(-26.0338171724679,-0.995597707882035,
2.33105492627659));
#6796=CARTESIAN_POINT('Ctrl Pts',(-25.9787262626427,-1.00008101774,2.32837603269168));
#6797=CARTESIAN_POINT('Ctrl Pts',(-25.8686962905678,-0.999917360916838,
2.32847915347901));
#6798=CARTESIAN_POINT('Ctrl Pts',(-25.8139981228264,-0.995338596268709,
2.33120606433384));
#6799=CARTESIAN_POINT('Ctrl Pts',(-25.6457369572167,-0.967153847373996,
2.34760035492244));
#6800=CARTESIAN_POINT('Ctrl Pts',(-25.5375353236883,-0.928753670997002,
2.36976707795446));
#6801=CARTESIAN_POINT('Ctrl Pts',(-25.3255406714161,-0.810864803746178,
2.42897889523381));
#6802=CARTESIAN_POINT('Ctrl Pts',(-25.2257850797809,-0.726489867907553,
2.46725895286448));
#6803=CARTESIAN_POINT('Ctrl Pts',(-25.0755270452453,-0.539171378438706,
2.53180070351187));
#6804=CARTESIAN_POINT('Ctrl Pts',(-25.0202559439199,-0.440786335109945,
2.558855638119));
#6805=CARTESIAN_POINT('Ctrl Pts',(-24.9446246649148,-0.227289219830435,
2.59695611074344));
#6806=CARTESIAN_POINT('Ctrl Pts',(-24.925,-0.114639026795822,2.60755684743755));
#6807=CARTESIAN_POINT('Ctrl Pts',(-24.925,6.24162981673305E-17,2.60755260924175));
#6808=CARTESIAN_POINT('Origin',(0.,0.,0.));
#6809=CARTESIAN_POINT('',(-19.525,-2.3,-2.81668763803891E-16));
#6810=CARTESIAN_POINT('Origin',(-19.525,8.93680102069846E-16,0.));
#6811=CARTESIAN_POINT('',(-20.325,-2.3,-2.81668763803891E-16));
#6812=CARTESIAN_POINT('',(-1.05273456325769E-16,-2.3,-2.81668763803891E-16));
#6813=CARTESIAN_POINT('Origin',(-20.325,9.30296956444027E-16,0.));
#6814=CARTESIAN_POINT('Origin',(28.225,1.03717240014867E-14,0.));
#6815=CARTESIAN_POINT('',(28.225,1.15,-1.40834381901944E-16));
#6816=CARTESIAN_POINT('Origin',(28.225,1.03717240014867E-14,0.));
#6817=CARTESIAN_POINT('',(28.425,0.949999999999984,-1.16341445918995E-16));
#6818=CARTESIAN_POINT('',(28.225,1.15,-1.40834381901944E-16));
#6819=CARTESIAN_POINT('Origin',(28.425,1.04083408558608E-14,0.));
#6820=CARTESIAN_POINT('Origin',(-28.425,0.,0.));
#6821=CARTESIAN_POINT('',(23.575,1.15,-1.40834381901944E-16));
#6822=CARTESIAN_POINT('Origin',(23.575,9.52038213728696E-15,0.));
#6823=CARTESIAN_POINT('',(-28.425,1.14999999999999,-1.40834381901944E-16));
#6824=CARTESIAN_POINT('Origin',(-28.425,0.,0.));
#6825=CARTESIAN_POINT('',(6.975,1.5,-1.83697019872102E-16));
#6826=CARTESIAN_POINT('Origin',(6.975,6.48118322422997E-15,0.));
#6827=CARTESIAN_POINT('',(23.575,1.5,-1.83697019872102E-16));
#6828=CARTESIAN_POINT('',(-28.425,1.49999999999999,-1.83697019872102E-16));
#6829=CARTESIAN_POINT('Origin',(23.575,9.52038213728696E-15,0.));
#6830=CARTESIAN_POINT('Origin',(6.975,6.48118322422997E-15,0.));
#6831=CARTESIAN_POINT('',(1.875,2.5,-3.06161699786838E-16));
#6832=CARTESIAN_POINT('Origin',(1.875,5.54745343768837E-15,0.));
#6833=CARTESIAN_POINT('',(6.975,2.,-2.4492935982947E-16));
#6834=CARTESIAN_POINT('',(6.975,2.,-2.4492935982947E-16));
#6835=CARTESIAN_POINT('Origin',(6.975,6.48118322422997E-15,0.));
#6836=CARTESIAN_POINT('Origin',(-28.425,0.,0.));
#6837=CARTESIAN_POINT('',(-19.525,3.,-3.67394039744206E-16));
#6838=CARTESIAN_POINT('Origin',(-19.525,8.93680102069846E-16,0.));
#6839=CARTESIAN_POINT('',(1.875,3.,-3.67394039744206E-16));
#6840=CARTESIAN_POINT('',(-28.425,3.,-3.67394039744206E-16));
#6841=CARTESIAN_POINT('Origin',(1.875,5.54745343768837E-15,0.));
#6842=CARTESIAN_POINT('Origin',(1.875,3.,0.));
#6843=CARTESIAN_POINT('Origin',(6.975,2.,0.));
#6844=CARTESIAN_POINT('Origin',(23.575,1.5,0.));
#6845=CARTESIAN_POINT('Origin',(28.425,1.15,0.));
#6846=CARTESIAN_POINT('Origin',(-20.325,-3.,0.));
#6847=CARTESIAN_POINT('Origin',(-19.525,-3.,0.));
#6848=CARTESIAN_POINT('Ctrl Pts',(-24.7512201965622,-1.76183904791747E-16,
3.00000124311957));
#6849=CARTESIAN_POINT('Ctrl Pts',(-24.7512206151827,-0.0224904615946165,
3.00000102486114));
#6850=CARTESIAN_POINT('Ctrl Pts',(-24.7517085809449,-0.0449131097845628,
2.99974818887592));
#6851=CARTESIAN_POINT('Ctrl Pts',(-24.7536439761057,-0.0895752885321344,
2.99874684907646));
#6852=CARTESIAN_POINT('Ctrl Pts',(-24.7550910425168,-0.111823263408201,
2.99799854559508));
#6853=CARTESIAN_POINT('Ctrl Pts',(-24.7608541223484,-0.1783210198246,2.99502561769244));
#6854=CARTESIAN_POINT('Ctrl Pts',(-24.7665915611397,-0.222335311776171,
2.99207181620778));
#6855=CARTESIAN_POINT('Ctrl Pts',(-24.7780288192454,-0.287837360410401,
2.98624162780084));
#6856=CARTESIAN_POINT('Ctrl Pts',(-24.7823197307722,-0.309606561385091,
2.9840619482597));
#6857=CARTESIAN_POINT('Ctrl Pts',(-24.7894679779366,-0.342109798413635,
2.98045092915735));
#6858=CARTESIAN_POINT('Ctrl Pts',(-24.7919724393738,-0.352930055186467,
2.97918882741414));
#6859=CARTESIAN_POINT('Ctrl Pts',(-24.7972214032702,-0.374523340751585,
2.97655141398561));
#6860=CARTESIAN_POINT('Ctrl Pts',(-24.7999681707864,-0.385302896814476,
2.97517498996412));
#6861=CARTESIAN_POINT('Ctrl Pts',(-24.8085247289755,-0.417396325006835,
2.97090101111401));
#6862=CARTESIAN_POINT('Ctrl Pts',(-24.8146611612218,-0.438519664833829,
2.96785340267611));
#6863=CARTESIAN_POINT('Ctrl Pts',(-24.827780795185,-0.480245605735743,2.96138777142348));
#6864=CARTESIAN_POINT('Ctrl Pts',(-24.8347634091537,-0.500846985261598,
2.95797002138279));
#6865=CARTESIAN_POINT('Ctrl Pts',(-24.8569585745012,-0.561885306302581,
2.94720211826449));
#6866=CARTESIAN_POINT('Ctrl Pts',(-24.8734157851973,-0.601558415893414,
2.93933707448591));
#6867=CARTESIAN_POINT('Ctrl Pts',(-24.9005699650057,-0.659577946472712,
2.92666307786021));
#6868=CARTESIAN_POINT('Ctrl Pts',(-24.9100343005407,-0.678670330222981,
2.92229185258577));
#6869=CARTESIAN_POINT('Ctrl Pts',(-24.9297925040438,-0.71635605219561,2.91328291034591));
#6870=CARTESIAN_POINT('Ctrl Pts',(-24.9400941970776,-0.734962854491018,
2.90864166879988));
#6871=CARTESIAN_POINT('Ctrl Pts',(-24.9615143509208,-0.771630108002665,
2.8991297911222));
#6872=CARTESIAN_POINT('Ctrl Pts',(-24.9725542617936,-0.789558390564698,
2.89429401664935));
#6873=CARTESIAN_POINT('Ctrl Pts',(-24.9953081681755,-0.824675412874891,
2.88448450367961));
#6874=CARTESIAN_POINT('Ctrl Pts',(-25.0070176561689,-0.841856330313478,
2.87951274183948));
#6875=CARTESIAN_POINT('Ctrl Pts',(-25.0431332882325,-0.892293349065707,
2.86444629839692));
#6876=CARTESIAN_POINT('Ctrl Pts',(-25.0685240643679,-0.92444624815415,2.85419987571196));
#6877=CARTESIAN_POINT('Ctrl Pts',(-25.1085917532924,-0.970519332950307,
2.83872559859403));
#6878=CARTESIAN_POINT('Ctrl Pts',(-25.1222785365167,-0.985516952511357,
2.83355000263622));
#6879=CARTESIAN_POINT('Ctrl Pts',(-25.1503245087481,-1.0147915600932,2.82319808714425));
#6880=CARTESIAN_POINT('Ctrl Pts',(-25.1646905450052,-1.02907433729268,2.81801945772866));
#6881=CARTESIAN_POINT('Ctrl Pts',(-25.1940839460452,-1.05688985201168,2.80770598732435));
#6882=CARTESIAN_POINT('Ctrl Pts',(-25.2091788350748,-1.07047868451993,2.80254912945966));
#6883=CARTESIAN_POINT('Ctrl Pts',(-25.2397857985023,-1.09666875082295,2.79240445901191));
#6884=CARTESIAN_POINT('Ctrl Pts',(-25.255320223101,-1.10929658351522,2.78740768552752));
#6885=CARTESIAN_POINT('Ctrl Pts',(-25.2868469170525,-1.13362940492584,2.77760057560582));
#6886=CARTESIAN_POINT('Ctrl Pts',(-25.302839623016,-1.14533536930589,2.77278994432858));
#6887=CARTESIAN_POINT('Ctrl Pts',(-25.3352860491081,-1.16783592991971,2.76338858760642));
#6888=CARTESIAN_POINT('Ctrl Pts',(-25.3517397751987,-1.17863049873125,2.75879782839759));
#6889=CARTESIAN_POINT('Ctrl Pts',(-25.4018014264425,-1.20964993058026,2.74540766718039));
#6890=CARTESIAN_POINT('Ctrl Pts',(-25.4361157965431,-1.22851722530086,2.7369879943305));
#6891=CARTESIAN_POINT('Ctrl Pts',(-25.4890319606085,-1.25402748115622,2.72534609489846));
#6892=CARTESIAN_POINT('Ctrl Pts',(-25.5069294362475,-1.26207118462111,2.72162720547797));
#6893=CARTESIAN_POINT('Ctrl Pts',(-25.5341341065867,-1.27341479768989,2.71632858891394));
#6894=CARTESIAN_POINT('Ctrl Pts',(-25.5432727036745,-1.27707929627404,2.71460725980808));
#6895=CARTESIAN_POINT('Ctrl Pts',(-25.5616696134459,-1.28416319515221,2.71126336921716));
#6896=CARTESIAN_POINT('Ctrl Pts',(-25.5709426986925,-1.28758734347613,2.70963852456332));
#6897=CARTESIAN_POINT('Ctrl Pts',(-25.5987920948568,-1.29743244195315,2.70494558321287));
#6898=CARTESIAN_POINT('Ctrl Pts',(-25.617433882299,-1.30344363716717,2.70205116137013));
#6899=CARTESIAN_POINT('Ctrl Pts',(-25.6548879621502,-1.31438372733535,2.69674641877482));
#6900=CARTESIAN_POINT('Ctrl Pts',(-25.6736968490448,-1.31931173160548,2.69433651551851));
#6901=CARTESIAN_POINT('Ctrl Pts',(-25.7303690237763,-1.33248274213305,2.68786059982172));
#6902=CARTESIAN_POINT('Ctrl Pts',(-25.7684773832559,-1.33911643529056,2.6845486252675));
#6903=CARTESIAN_POINT('Ctrl Pts',(-25.8261391213393,-1.34582410918546,2.68118864483476));
#6904=CARTESIAN_POINT('Ctrl Pts',(-25.8454430068625,-1.34751862690545,2.68033657178926));
#6905=CARTESIAN_POINT('Ctrl Pts',(-25.8842203794928,-1.34980853567155,2.67918411053143));
#6906=CARTESIAN_POINT('Ctrl Pts',(-25.9037051371427,-1.35040321450496,2.67888411665589));
#6907=CARTESIAN_POINT('Ctrl Pts',(-25.9428031440834,-1.35047173299045,2.67884957398269));
#6908=CARTESIAN_POINT('Ctrl Pts',(-25.9625262788923,-1.34993763378488,2.67911903945913));
#6909=CARTESIAN_POINT('Ctrl Pts',(-26.001675179068,-1.34774256849848,2.68022395142751));
#6910=CARTESIAN_POINT('Ctrl Pts',(-26.0211401464231,-1.34608753889995,2.68105638390197));
#6911=CARTESIAN_POINT('Ctrl Pts',(-26.0598521561959,-1.34168374443805,2.68326288816889));
#6912=CARTESIAN_POINT('Ctrl Pts',(-26.0790999491839,-1.33893558390626,2.68463664029074));
#6913=CARTESIAN_POINT('Ctrl Pts',(-26.1173832731121,-1.33236285214624,2.68790468740719));
#6914=CARTESIAN_POINT('Ctrl Pts',(-26.1364187960914,-1.3285382337657,2.6897989878991));
#6915=CARTESIAN_POINT('Ctrl Pts',(-26.1932112333693,-1.31546132541517,2.69623160867151));
#6916=CARTESIAN_POINT('Ctrl Pts',(-26.230658868257,-1.30460568802834,2.70152164206104));
#6917=CARTESIAN_POINT('Ctrl Pts',(-26.2769394358952,-1.28835579481113,2.70927322407079));
#6918=CARTESIAN_POINT('Ctrl Pts',(-26.2861736873588,-1.28496804550343,2.71088197061785));
#6919=CARTESIAN_POINT('Ctrl Pts',(-26.3045801226384,-1.27792632816734,2.71420859259991));
#6920=CARTESIAN_POINT('Ctrl Pts',(-26.3137696612827,-1.27426435838069,2.71593014837302));
#6921=CARTESIAN_POINT('Ctrl Pts',(-26.3411343470425,-1.26292005406289,2.72123342520569));
#6922=CARTESIAN_POINT('Ctrl Pts',(-26.3591086288947,-1.25488236548527,2.72495256846718));
#6923=CARTESIAN_POINT('Ctrl Pts',(-26.3945730991822,-1.23786441433935,2.73272536195925));
#6924=CARTESIAN_POINT('Ctrl Pts',(-26.4120574252086,-1.22888679609906,2.73677778918298));
#6925=CARTESIAN_POINT('Ctrl Pts',(-26.4465443911629,-1.21000870437874,2.74517655409933));
#6926=CARTESIAN_POINT('Ctrl Pts',(-26.4635470144595,-1.20010820517651,2.74952291627504));
#6927=CARTESIAN_POINT('Ctrl Pts',(-26.4970806133762,-1.17939058963319,2.75847308374743));
#6928=CARTESIAN_POINT('Ctrl Pts',(-26.5136115807888,-1.16857346524795,2.76307691198199));
#6929=CARTESIAN_POINT('Ctrl Pts',(-26.5462080833809,-1.14602103189425,2.77250675337683));
#6930=CARTESIAN_POINT('Ctrl Pts',(-26.5622736983626,-1.1342856634169,2.77733281570969));
#6931=CARTESIAN_POINT('Ctrl Pts',(-26.5939416429695,-1.10988763337467,2.78717256703881));
#6932=CARTESIAN_POINT('Ctrl Pts',(-26.609547564207,-1.09722193187051,2.79218745199254));
#6933=CARTESIAN_POINT('Ctrl Pts',(-26.6402813438902,-1.07095721724289,2.8023664037371));
#6934=CARTESIAN_POINT('Ctrl Pts',(-26.655295080658,-1.05745634546246,2.80749236059604));
#6935=CARTESIAN_POINT('Ctrl Pts',(-26.6846548548111,-1.02971401041123,2.81778570291711));
#6936=CARTESIAN_POINT('Ctrl Pts',(-26.698997953854,-1.01547501212971,2.82295214467571));
#6937=CARTESIAN_POINT('Ctrl Pts',(-26.7270253212179,-0.9862662210335,2.83328911051859));
#6938=CARTESIAN_POINT('Ctrl Pts',(-26.7407095447861,-0.971296396677904,
2.83845969056953));
#6939=CARTESIAN_POINT('Ctrl Pts',(-26.7807872610901,-0.925288863725475,
2.85392633511737));
#6940=CARTESIAN_POINT('Ctrl Pts',(-26.8062107356642,-0.893151941339901,
2.864178670324));
#6941=CARTESIAN_POINT('Ctrl Pts',(-26.8423947744529,-0.842704579251605,
2.87926472137709));
#6942=CARTESIAN_POINT('Ctrl Pts',(-26.8541358893937,-0.825504953419079,
2.88424727122285));
#6943=CARTESIAN_POINT('Ctrl Pts',(-26.8712465648999,-0.799139107619217,
2.89162033090013));
#6944=CARTESIAN_POINT('Ctrl Pts',(-26.8768710845513,-0.790248327529814,
2.89406322620423));
#6945=CARTESIAN_POINT('Ctrl Pts',(-26.8879472162261,-0.772282090199619,
2.89890928529195));
#6946=CARTESIAN_POINT('Ctrl Pts',(-26.8934095805383,-0.763187949365317,
2.9013172405501));
#6947=CARTESIAN_POINT('Ctrl Pts',(-26.9094752397211,-0.735724969537462,
2.90844874441802));
#6948=CARTESIAN_POINT('Ctrl Pts',(-26.9197553059395,-0.717185246436077,
2.91307852354811));
#6949=CARTESIAN_POINT('Ctrl Pts',(-26.939491662068,-0.679606241243712,2.92207399934037));
#6950=CARTESIAN_POINT('Ctrl Pts',(-26.9489441843561,-0.660573675186057,
2.92643805302077));
#6951=CARTESIAN_POINT('Ctrl Pts',(-26.9760664924627,-0.602745972669873,
2.93909208245404));
#6952=CARTESIAN_POINT('Ctrl Pts',(-26.9925039932974,-0.563222492320479,
2.94694446393472));
#6953=CARTESIAN_POINT('Ctrl Pts',(-27.0220719282814,-0.482184935663518,
2.96128319208414));
#6954=CARTESIAN_POINT('Ctrl Pts',(-27.0352038812473,-0.440658278132651,
2.96777086803717));
#6955=CARTESIAN_POINT('Ctrl Pts',(-27.0523220500515,-0.376834051179656,
2.97631783456127));
#6956=CARTESIAN_POINT('Ctrl Pts',(-27.0576008937577,-0.355274612711083,
2.97897112077082));
#6957=CARTESIAN_POINT('Ctrl Pts',(-27.0672604256937,-0.311662928430509,
2.98384906046174));
#6958=CARTESIAN_POINT('Ctrl Pts',(-27.0716118507556,-0.28974195783202,2.98605887165636));
#6959=CARTESIAN_POINT('Ctrl Pts',(-27.0793664061891,-0.245626216202856,
2.99001098961276));
#6960=CARTESIAN_POINT('Ctrl Pts',(-27.0827665013565,-0.223449220869781,
2.99175175446374));
#6961=CARTESIAN_POINT('Ctrl Pts',(-27.0886129441394,-0.178789236716059,
2.99475258363014));
#6962=CARTESIAN_POINT('Ctrl Pts',(-27.0910452438611,-0.15640475955994,2.99600543335325));
#6963=CARTESIAN_POINT('Ctrl Pts',(-27.0968540554839,-0.089380072836346,
2.99900191231137));
#6964=CARTESIAN_POINT('Ctrl Pts',(-27.0987766251388,-0.0447217917816824,
2.99999958185766));
#6965=CARTESIAN_POINT('Ctrl Pts',(-27.0987813865579,0.02219325478624,3.00000207062791));
#6966=CARTESIAN_POINT('Ctrl Pts',(-27.098302980501,0.0444882044529776,2.99975417679133));
#6967=CARTESIAN_POINT('Ctrl Pts',(-27.0963851499708,0.0890579606384697,
2.99876191230976));
#6968=CARTESIAN_POINT('Ctrl Pts',(-27.0949457527391,0.111332767632207,2.99801754221172));
#6969=CARTESIAN_POINT('Ctrl Pts',(-27.091097912228,0.155862099946067,2.99603257401337));
#6970=CARTESIAN_POINT('Ctrl Pts',(-27.0886882785475,0.178121325914285,2.99479136150237));
#6971=CARTESIAN_POINT('Ctrl Pts',(-27.0828893311938,0.222600421497831,2.99181469259339));
#6972=CARTESIAN_POINT('Ctrl Pts',(-27.0794844211542,0.244888534479486,2.99007132802239));
#6973=CARTESIAN_POINT('Ctrl Pts',(-27.0717763207677,0.288870061738483,2.98614250919086));
#6974=CARTESIAN_POINT('Ctrl Pts',(-27.0674611935747,0.310670506014752,2.98395091125391));
#6975=CARTESIAN_POINT('Ctrl Pts',(-27.0579367437935,0.353839565051259,2.9791402804281));
#6976=CARTESIAN_POINT('Ctrl Pts',(-27.0527261874502,0.375218601036114,2.97652060572815));
#6977=CARTESIAN_POINT('Ctrl Pts',(-27.0357699204893,0.438751951157216,2.96805162738344));
#6978=CARTESIAN_POINT('Ctrl Pts',(-27.022699391642,0.480310643319706,2.9615908339538));
#6979=CARTESIAN_POINT('Ctrl Pts',(-27.0004758229384,0.541446694763495,2.95080875849622));
#6980=CARTESIAN_POINT('Ctrl Pts',(-26.992623681753,0.561640072316629,2.94702942050088));
#6981=CARTESIAN_POINT('Ctrl Pts',(-26.9801909795193,0.591614335345463,2.94110596088858));
#6982=CARTESIAN_POINT('Ctrl Pts',(-26.9759332605878,0.60156226518298,2.9390870305072));
#6983=CARTESIAN_POINT('Ctrl Pts',(-26.9671990237161,0.621350626541985,2.9349673711246));
#6984=CARTESIAN_POINT('Ctrl Pts',(-26.9627163520765,0.631203409825238,2.93286380405279));
#6985=CARTESIAN_POINT('Ctrl Pts',(-26.9490003388169,0.660466615132205,2.92646369421333));
#6986=CARTESIAN_POINT('Ctrl Pts',(-26.9394866261483,0.679617007741926,2.92207164107701));
#6987=CARTESIAN_POINT('Ctrl Pts',(-26.9197263731453,0.717239156030636,2.91306539958487));
#6988=CARTESIAN_POINT('Ctrl Pts',(-26.9094813066202,0.735708225799572,2.9084518514383));
#6989=CARTESIAN_POINT('Ctrl Pts',(-26.8776651907974,0.790114397662365,2.89432752559281));
#6990=CARTESIAN_POINT('Ctrl Pts',(-26.855015951808,0.825052668578728,2.88453262436396));
#6991=CARTESIAN_POINT('Ctrl Pts',(-26.8188828130475,0.875511458559016,2.86945918682943));
#6992=CARTESIAN_POINT('Ctrl Pts',(-26.806477865951,0.892005672721574,2.86437109863276));
#6993=CARTESIAN_POINT('Ctrl Pts',(-26.7809370903558,0.924343794681297,2.85409960048903));
#6994=CARTESIAN_POINT('Ctrl Pts',(-26.7678062754663,0.94018178468473,2.84891809889914));
#6995=CARTESIAN_POINT('Ctrl Pts',(-26.747534952965,0.963465362975877,2.8410930742898));
#6996=CARTESIAN_POINT('Ctrl Pts',(-26.7406847515848,0.971143336910766,2.83847720905191));
#6997=CARTESIAN_POINT('Ctrl Pts',(-26.726866828362,0.986257778221377,2.8332609577602));
#6998=CARTESIAN_POINT('Ctrl Pts',(-26.7198864405152,0.993708965489587,2.83065565931379));
#6999=CARTESIAN_POINT('Ctrl Pts',(-26.6987545667654,1.01572267126073,2.82286342050641));
#7000=CARTESIAN_POINT('Ctrl Pts',(-26.6843929425923,1.02996804274084,2.81769254606288));
#7001=CARTESIAN_POINT('Ctrl Pts',(-26.6405196961263,1.07140451601384,2.80231490014364));
#7002=CARTESIAN_POINT('Ctrl Pts',(-26.6101990167324,1.09732522138671,2.79223355729096));
#7003=CARTESIAN_POINT('Ctrl Pts',(-26.5630920876351,1.13367314163991,2.77758248050925));
#7004=CARTESIAN_POINT('Ctrl Pts',(-26.5471176954077,1.14536678978723,2.77277705423988));
#7005=CARTESIAN_POINT('Ctrl Pts',(-26.5146128603087,1.16790420277309,2.76335982199196));
#7006=CARTESIAN_POINT('Ctrl Pts',(-26.4980824626504,1.17874802188457,2.75874796251914));
#7007=CARTESIAN_POINT('Ctrl Pts',(-26.4644489769846,1.19957326674856,2.74975657993441));
#7008=CARTESIAN_POINT('Ctrl Pts',(-26.4473526605441,1.20955077156384,2.74537877233407));
#7009=CARTESIAN_POINT('Ctrl Pts',(-26.4212418428209,1.22386659438305,2.73901196687352));
#7010=CARTESIAN_POINT('Ctrl Pts',(-26.4124621517901,1.228528090482,2.73692383614117));
#7011=CARTESIAN_POINT('Ctrl Pts',(-26.3948579023758,1.23757356026446,2.73284557774276));
#7012=CARTESIAN_POINT('Ctrl Pts',(-26.3860148872854,1.24196849424176,2.73085066873684));
#7013=CARTESIAN_POINT('Ctrl Pts',(-26.341645261955,1.26327266721299,2.72112112107028));
#7014=CARTESIAN_POINT('Ctrl Pts',(-26.3055755853367,1.27824593843012,2.71409299783002));
#7015=CARTESIAN_POINT('Ctrl Pts',(-26.2323061069552,1.30408058177653,2.70177489330743));
#7016=CARTESIAN_POINT('Ctrl Pts',(-26.1951017095151,1.31494712049099,2.69648267860914));
#7017=CARTESIAN_POINT('Ctrl Pts',(-26.1384101250037,1.32811617463851,2.69000746444321));
#7018=CARTESIAN_POINT('Ctrl Pts',(-26.1193652332726,1.33198320784822,2.68809291154564));
#7019=CARTESIAN_POINT('Ctrl Pts',(-26.0809718851876,1.3386498031086,2.68477922262698));
#7020=CARTESIAN_POINT('Ctrl Pts',(-26.0616267484912,1.34144867007465,2.68338047067986));
#7021=CARTESIAN_POINT('Ctrl Pts',(-26.032363761062,1.34482540214699,2.68168886075706));
#7022=CARTESIAN_POINT('Ctrl Pts',(-26.0225572765905,1.34581398544558,2.6811927471385));
#7023=CARTESIAN_POINT('Ctrl Pts',(-26.0029866880182,1.34750220702749,2.68034468497323));
#7024=CARTESIAN_POINT('Ctrl Pts',(-25.9932072525691,1.34820413161832,2.67999159504196));
#7025=CARTESIAN_POINT('Ctrl Pts',(-25.9639248763077,1.34988314454028,2.6791465090366));
#7026=CARTESIAN_POINT('Ctrl Pts',(-25.944430256616,1.35043954651561,2.67886577671177));
#7027=CARTESIAN_POINT('Ctrl Pts',(-25.8861245439706,1.3504378095549,2.67886672345498));
#7028=CARTESIAN_POINT('Ctrl Pts',(-25.8474103812661,1.34822168461923,2.67998726078285));
#7029=CARTESIAN_POINT('Ctrl Pts',(-25.7896108997839,1.34161043104656,2.68329952853649));
#7030=CARTESIAN_POINT('Ctrl Pts',(-25.77038745646,1.33885814096473,2.68467529043326));
#7031=CARTESIAN_POINT('Ctrl Pts',(-25.7320267290187,1.33225068682402,2.68796030874541));
#7032=CARTESIAN_POINT('Ctrl Pts',(-25.7128830247106,1.32839365293775,2.68987049972103));
#7033=CARTESIAN_POINT('Ctrl Pts',(-25.684251748041,1.32177623227189,2.69312505274073));
#7034=CARTESIAN_POINT('Ctrl Pts',(-25.6747141290368,1.31942923189441,2.69427597594583));
#7035=CARTESIAN_POINT('Ctrl Pts',(-25.6556602502347,1.31445363734784,2.69670691417443));
#7036=CARTESIAN_POINT('Ctrl Pts',(-25.6461499439873,1.31182592199724,2.69798646989669));
#7037=CARTESIAN_POINT('Ctrl Pts',(-25.6178199688841,1.30356690507148,2.70199177974632));
#7038=CARTESIAN_POINT('Ctrl Pts',(-25.5991462839436,1.29754850153216,2.7048898077093));
#7039=CARTESIAN_POINT('Ctrl Pts',(-25.5622141869212,1.28451064624858,2.71110556040655));
#7040=CARTESIAN_POINT('Ctrl Pts',(-25.5439551422566,1.27749140423903,2.71442318809091));
#7041=CARTESIAN_POINT('Ctrl Pts',(-25.5078398888184,1.26246846951838,2.7214427902055));
#7042=CARTESIAN_POINT('Ctrl Pts',(-25.4899837037464,1.25446472257528,2.72514479532609));
#7043=CARTESIAN_POINT('Ctrl Pts',(-25.4370072942282,1.22898847560418,2.73677631458511));
#7044=CARTESIAN_POINT('Ctrl Pts',(-25.4024760017176,1.21005101589909,2.74523245622064));
#7045=CARTESIAN_POINT('Ctrl Pts',(-25.3602838735484,1.18392877826526,2.75651122868636));
#7046=CARTESIAN_POINT('Ctrl Pts',(-25.3518919706823,1.17857845856369,2.75880349026457));
#7047=CARTESIAN_POINT('Ctrl Pts',(-25.3352100824015,1.16763411776591,2.76345337348231));
#7048=CARTESIAN_POINT('Ctrl Pts',(-25.3269100051743,1.16203215951806,2.76581417940247));
#7049=CARTESIAN_POINT('Ctrl Pts',(-25.3022695725318,1.14493024612509,2.77295794310452));
#7050=CARTESIAN_POINT('Ctrl Pts',(-25.2861657292169,1.13312260725419,2.77780759607733));
#7051=CARTESIAN_POINT('Ctrl Pts',(-25.2545675218788,1.10869580205534,2.78764693628012));
#7052=CARTESIAN_POINT('Ctrl Pts',(-25.2390758775543,1.09607878865392,2.7926357760188));
#7053=CARTESIAN_POINT('Ctrl Pts',(-25.208692728647,1.07004449005284,2.80271440082356));
#7054=CARTESIAN_POINT('Ctrl Pts',(-25.193801243974,1.05662718870003,2.80780421768086));
#7055=CARTESIAN_POINT('Ctrl Pts',(-25.1646090505302,1.02899230331321,2.81804902565378));
#7056=CARTESIAN_POINT('Ctrl Pts',(-25.150308350114,1.0147747185966,2.82320404678685));
#7057=CARTESIAN_POINT('Ctrl Pts',(-25.1222934624824,0.985532507337768,2.83354449797841));
#7058=CARTESIAN_POINT('Ctrl Pts',(-25.1085792726074,0.970507895413088,2.83872995787953));
#7059=CARTESIAN_POINT('Ctrl Pts',(-25.0817381947277,0.939637998238792,2.84909699750195));
#7060=CARTESIAN_POINT('Ctrl Pts',(-25.0686119208846,0.923793044275968,2.8542784068245));
#7061=CARTESIAN_POINT('Ctrl Pts',(-25.0493655924709,0.89939352728851,2.86202245059147));
#7062=CARTESIAN_POINT('Ctrl Pts',(-25.0430172047533,0.891144919357543,2.86460202126226));
#7063=CARTESIAN_POINT('Ctrl Pts',(-25.0305204210295,0.874501923571608,2.86972650110557));
#7064=CARTESIAN_POINT('Ctrl Pts',(-25.02437110194,0.866107944767956,2.87227157889308));
#7065=CARTESIAN_POINT('Ctrl Pts',(-24.9941173036171,0.823768140450452,2.88490209785398));
#7066=CARTESIAN_POINT('Ctrl Pts',(-24.971471952131,0.788729223015757,2.89470441040782));
#7067=CARTESIAN_POINT('Ctrl Pts',(-24.9292309034491,0.716312201964233,2.91346931208067));
#7068=CARTESIAN_POINT('Ctrl Pts',(-24.9096333854723,0.67893485651281,2.92243312349527));
#7069=CARTESIAN_POINT('Ctrl Pts',(-24.882541170584,0.621060652496465,2.93507771188247));
#7070=CARTESIAN_POINT('Ctrl Pts',(-24.8738951241542,0.601467423657377,2.93915911726366));
#7071=CARTESIAN_POINT('Ctrl Pts',(-24.8573856909762,0.561660850722054,2.94702500788258));
#7072=CARTESIAN_POINT('Ctrl Pts',(-24.8495218895994,0.541445422596672,2.95080973422482));
#7073=CARTESIAN_POINT('Ctrl Pts',(-24.8383292807319,0.510647491444322,2.95624018705409));
#7074=CARTESIAN_POINT('Ctrl Pts',(-24.8346940039926,0.500285853504753,2.95801168194031));
#7075=CARTESIAN_POINT('Ctrl Pts',(-24.8276504459147,0.47946808360172,2.96145728412088));
#7076=CARTESIAN_POINT('Ctrl Pts',(-24.8242483365591,0.469031804392166,2.96312833452968));
#7077=CARTESIAN_POINT('Ctrl Pts',(-24.8143971656437,0.43763579155551,2.96798415471264));
#7078=CARTESIAN_POINT('Ctrl Pts',(-24.8082915227193,0.416559647886907,2.97101715178475));
#7079=CARTESIAN_POINT('Ctrl Pts',(-24.7970093173975,0.374165786036183,2.97665328568467));
#7080=CARTESIAN_POINT('Ctrl Pts',(-24.7918298385069,0.352840123671072,2.97925785882102));
#7081=CARTESIAN_POINT('Ctrl Pts',(-24.782389163039,0.309931323851521,2.98402682340998));
#7082=CARTESIAN_POINT('Ctrl Pts',(-24.7781279721287,0.288348186260506,2.98619122824603));
#7083=CARTESIAN_POINT('Ctrl Pts',(-24.7705258708633,0.244922725747236,2.99006614582328));
#7084=CARTESIAN_POINT('Ctrl Pts',(-24.7671849516661,0.223080406167033,2.99177667236476));
#7085=CARTESIAN_POINT('Ctrl Pts',(-24.7614323434624,0.179133152105929,2.99472933868235));
#7086=CARTESIAN_POINT('Ctrl Pts',(-24.7590206303916,0.157028224677869,2.99597149337493));
#7087=CARTESIAN_POINT('Ctrl Pts',(-24.7551426261223,0.112550514170608,2.99797188287434));
#7088=CARTESIAN_POINT('Ctrl Pts',(-24.7536766612853,0.0901766051585178,
2.99872994324477));
#7089=CARTESIAN_POINT('Ctrl Pts',(-24.7522036848644,0.056412851214161,2.99949202836053));
#7090=CARTESIAN_POINT('Ctrl Pts',(-24.7518340087419,0.045106917611639,2.9996834086165));
#7091=CARTESIAN_POINT('Ctrl Pts',(-24.751342340005,0.0225174807118006,2.99993797771742));
#7092=CARTESIAN_POINT('Ctrl Pts',(-24.751219987252,0.0112452307973078,3.00000135224878));
#7093=CARTESIAN_POINT('Ctrl Pts',(-24.7512201965622,-1.76183904791747E-16,
3.00000124311957));
#7094=CARTESIAN_POINT('Ctrl Pts',(-24.925001560524,1.55857043960029E-16,
2.60754908509522));
#7095=CARTESIAN_POINT('Ctrl Pts',(-24.9250019171665,-0.0166541334801613,
2.60754889538878));
#7096=CARTESIAN_POINT('Ctrl Pts',(-24.9254176382407,-0.0332580512905814,
2.60732913473253));
#7097=CARTESIAN_POINT('Ctrl Pts',(-24.9270664927659,-0.0663302887433916,
2.60645878753386));
#7098=CARTESIAN_POINT('Ctrl Pts',(-24.9282993169708,-0.0828048613803104,
2.60580837511734));
#7099=CARTESIAN_POINT('Ctrl Pts',(-24.9332091568075,-0.132046292319869,
2.6032243577104));
#7100=CARTESIAN_POINT('Ctrl Pts',(-24.9380971518304,-0.164638771132326,
2.60065696465499));
#7101=CARTESIAN_POINT('Ctrl Pts',(-24.9478410920693,-0.2131428828209,2.59558946593898));
#7102=CARTESIAN_POINT('Ctrl Pts',(-24.9514967222119,-0.229262924518058,
2.59369492625983));
#7103=CARTESIAN_POINT('Ctrl Pts',(-24.957586651506,-0.253331494462499,2.59055629104135));
#7104=CARTESIAN_POINT('Ctrl Pts',(-24.9597203204629,-0.261343868943599,
2.58945929408072));
#7105=CARTESIAN_POINT('Ctrl Pts',(-24.9641921606581,-0.277333645699326,
2.58716690003975));
#7106=CARTESIAN_POINT('Ctrl Pts',(-24.9665322616052,-0.285315881401586,
2.58597053613621));
#7107=CARTESIAN_POINT('Ctrl Pts',(-24.9738219975603,-0.309080988873579,
2.58225566779538));
#7108=CARTESIAN_POINT('Ctrl Pts',(-24.9790499139481,-0.324722771924263,
2.57960673936175));
#7109=CARTESIAN_POINT('Ctrl Pts',(-24.9902271496198,-0.355620732215222,
2.57398692473798));
#7110=CARTESIAN_POINT('Ctrl Pts',(-24.9961759681728,-0.370876004900204,
2.57101627563854));
#7111=CARTESIAN_POINT('Ctrl Pts',(-25.015085077571,-0.416074736889795,2.5616570008748));
#7112=CARTESIAN_POINT('Ctrl Pts',(-25.0291057524579,-0.445452580460472,
2.55482084113838));
#7113=CARTESIAN_POINT('Ctrl Pts',(-25.0522396804357,-0.488415905271011,
2.54380482293415));
#7114=CARTESIAN_POINT('Ctrl Pts',(-25.060302794776,-0.502553770162814,2.54000542968693));
#7115=CARTESIAN_POINT('Ctrl Pts',(-25.0771357413066,-0.530459957917378,
2.53217501323324));
#7116=CARTESIAN_POINT('Ctrl Pts',(-25.0859122400396,-0.54423825089383,2.5281409265225));
#7117=CARTESIAN_POINT('Ctrl Pts',(-25.1041610805409,-0.571390265168159,
2.51987336730303));
#7118=CARTESIAN_POINT('Ctrl Pts',(-25.113566501909,-0.584666115891092,2.51567019594392));
#7119=CARTESIAN_POINT('Ctrl Pts',(-25.1329516291768,-0.610670187636849,
2.50714393728714));
#7120=CARTESIAN_POINT('Ctrl Pts',(-25.1429274949106,-0.623392616257929,
2.50282256806535));
#7121=CARTESIAN_POINT('Ctrl Pts',(-25.1736961072169,-0.660741109040536,
2.48972707655347));
#7122=CARTESIAN_POINT('Ctrl Pts',(-25.195327708338,-0.68455025456915,2.48082106354484));
#7123=CARTESIAN_POINT('Ctrl Pts',(-25.2294632644966,-0.718667264605278,
2.46737109007097));
#7124=CARTESIAN_POINT('Ctrl Pts',(-25.2411236814041,-0.729772966325544,
2.46287255176686));
#7125=CARTESIAN_POINT('Ctrl Pts',(-25.2650173694561,-0.751450743819418,
2.45387484623857));
#7126=CARTESIAN_POINT('Ctrl Pts',(-25.2772564740961,-0.762027106466302,
2.44937367130548));
#7127=CARTESIAN_POINT('Ctrl Pts',(-25.3022981003744,-0.782624429154989,
2.44040938158115));
#7128=CARTESIAN_POINT('Ctrl Pts',(-25.3151581491073,-0.792686927403681,
2.43592713010271));
#7129=CARTESIAN_POINT('Ctrl Pts',(-25.3412336664868,-0.81208060939496,2.42710955837504));
#7130=CARTESIAN_POINT('Ctrl Pts',(-25.3544681763255,-0.821431489558622,
2.42276644946543));
#7131=CARTESIAN_POINT('Ctrl Pts',(-25.3813272555676,-0.839449886111459,
2.41424227949637));
#7132=CARTESIAN_POINT('Ctrl Pts',(-25.3949521969405,-0.848118124975917,
2.41006096216709));
#7133=CARTESIAN_POINT('Ctrl Pts',(-25.4225948394221,-0.864779736753649,
2.40188946584663));
#7134=CARTESIAN_POINT('Ctrl Pts',(-25.4366125456109,-0.872773089361171,
2.39789925750829));
#7135=CARTESIAN_POINT('Ctrl Pts',(-25.4792624301743,-0.895742905086398,
2.38626076145437));
#7136=CARTESIAN_POINT('Ctrl Pts',(-25.5084964623614,-0.909714092086863,
2.37894252774089));
#7137=CARTESIAN_POINT('Ctrl Pts',(-25.5535782411859,-0.928604376053514,
2.36882359052986));
#7138=CARTESIAN_POINT('Ctrl Pts',(-25.5688259457879,-0.934560719395051,
2.36559119630036));
#7139=CARTESIAN_POINT('Ctrl Pts',(-25.5920028890314,-0.942960637972592,
2.36098573061775));
#7140=CARTESIAN_POINT('Ctrl Pts',(-25.599788491408,-0.945674190484402,2.35948958119256));
#7141=CARTESIAN_POINT('Ctrl Pts',(-25.6154616875292,-0.950919800805243,
2.35658312944661));
#7142=CARTESIAN_POINT('Ctrl Pts',(-25.6233618667185,-0.95345537451926,2.35517084263494));
#7143=CARTESIAN_POINT('Ctrl Pts',(-25.6470880823364,-0.960745646595251,
2.35109181935035));
#7144=CARTESIAN_POINT('Ctrl Pts',(-25.6629699013087,-0.965196922396583,
2.3485760380501));
#7145=CARTESIAN_POINT('Ctrl Pts',(-25.6948788004851,-0.973298033223291,
2.34396524772702));
#7146=CARTESIAN_POINT('Ctrl Pts',(-25.7109029793721,-0.976947208699515,
2.34187060158446));
#7147=CARTESIAN_POINT('Ctrl Pts',(-25.7591846810364,-0.98670031076137,2.33624184790048));
#7148=CARTESIAN_POINT('Ctrl Pts',(-25.7916509919276,-0.991612544814396,
2.33336313702002));
#7149=CARTESIAN_POINT('Ctrl Pts',(-25.8407757493374,-0.996579561426912,
2.33044270026262));
#7150=CARTESIAN_POINT('Ctrl Pts',(-25.8572216409297,-0.997834347780394,
2.32970209313936));
#7151=CARTESIAN_POINT('Ctrl Pts',(-25.8902579157094,-0.999530019791506,
2.32870039378829));
#7152=CARTESIAN_POINT('Ctrl Pts',(-25.9068579008084,-0.999970378057432,
2.32843964431104));
#7153=CARTESIAN_POINT('Ctrl Pts',(-25.940167339092,-1.00002111583351,2.3284096204183));
#7154=CARTESIAN_POINT('Ctrl Pts',(-25.9569704089505,-0.999625616638187,
2.32864383514006));
#7155=CARTESIAN_POINT('Ctrl Pts',(-25.9903232055858,-0.998000175999123,
2.32960420547288));
#7156=CARTESIAN_POINT('Ctrl Pts',(-26.0069063303974,-0.996774630505924,
2.33032774135208));
#7157=CARTESIAN_POINT('Ctrl Pts',(-26.0398869194724,-0.993513631149867,
2.33224559661821));
#7158=CARTESIAN_POINT('Ctrl Pts',(-26.056285023184,-0.991478624792919,2.33343963815292));
#7159=CARTESIAN_POINT('Ctrl Pts',(-26.0889003945458,-0.986611532510906,
2.33628016806539));
#7160=CARTESIAN_POINT('Ctrl Pts',(-26.105117655415,-0.983779411669397,2.33792666122145));
#7161=CARTESIAN_POINT('Ctrl Pts',(-26.1535018144212,-0.974095992046507,
2.34351778370753));
#7162=CARTESIAN_POINT('Ctrl Pts',(-26.1854052228443,-0.966057418299631,
2.34811578904634));
#7163=CARTESIAN_POINT('Ctrl Pts',(-26.2248338237297,-0.954024410911544,
2.35485332977763));
#7164=CARTESIAN_POINT('Ctrl Pts',(-26.2327009185887,-0.951515790581753,
2.35625162439446));
#7165=CARTESIAN_POINT('Ctrl Pts',(-26.2483822299402,-0.946301415592757,
2.35914306656481));
#7166=CARTESIAN_POINT('Ctrl Pts',(-26.2562112318338,-0.943589735649563,
2.36063941300517));
#7167=CARTESIAN_POINT('Ctrl Pts',(-26.2795244997708,-0.935189305203641,
2.36524892931282));
#7168=CARTESIAN_POINT('Ctrl Pts',(-26.2948376392117,-0.929237415872055,
2.36848154417623));
#7169=CARTESIAN_POINT('Ctrl Pts',(-26.325051496053,-0.916635663404123,2.37523752156304));
#7170=CARTESIAN_POINT('Ctrl Pts',(-26.3399472189906,-0.90998775838627,2.37875982107005));
#7171=CARTESIAN_POINT('Ctrl Pts',(-26.3693282937335,-0.896008576234018,
2.3860598819696));
#7172=CARTESIAN_POINT('Ctrl Pts',(-26.3838136313699,-0.888677280052333,
2.38983766464245));
#7173=CARTESIAN_POINT('Ctrl Pts',(-26.4123824877163,-0.873335934871314,
2.39761699508693));
#7174=CARTESIAN_POINT('Ctrl Pts',(-26.426465999434,-0.865325879915252,2.40161856279578));
#7175=CARTESIAN_POINT('Ctrl Pts',(-26.4542364991725,-0.848625856496643,
2.40981481750003));
#7176=CARTESIAN_POINT('Ctrl Pts',(-26.4679235551807,-0.839935843967816,
2.41400954723539));
#7177=CARTESIAN_POINT('Ctrl Pts',(-26.4949029725259,-0.821869160578,2.42256208855009));
#7178=CARTESIAN_POINT('Ctrl Pts',(-26.508198393727,-0.812490238648981,2.42692093963487));
#7179=CARTESIAN_POINT('Ctrl Pts',(-26.5343819518632,-0.79304127975015,2.43576830807167));
#7180=CARTESIAN_POINT('Ctrl Pts',(-26.5471728631521,-0.783043916212123,
2.44022370093141));
#7181=CARTESIAN_POINT('Ctrl Pts',(-26.5721858410977,-0.762500782893491,
2.4491704956747));
#7182=CARTESIAN_POINT('Ctrl Pts',(-26.5844054044419,-0.751956838431768,
2.45366107730754));
#7183=CARTESIAN_POINT('Ctrl Pts',(-26.6082832421287,-0.730327797889394,
2.46264578885994));
#7184=CARTESIAN_POINT('Ctrl Pts',(-26.6199414783443,-0.719242678452863,
2.46713996742474));
#7185=CARTESIAN_POINT('Ctrl Pts',(-26.654085577301,-0.68517420940159,2.48058330680097));
#7186=CARTESIAN_POINT('Ctrl Pts',(-26.6757450357663,-0.661376894583312,
2.48949445887105));
#7187=CARTESIAN_POINT('Ctrl Pts',(-26.7065719269914,-0.624020742585236,
2.50260699297805));
#7188=CARTESIAN_POINT('Ctrl Pts',(-26.7165747372153,-0.611284460442826,
2.50693773894737));
#7189=CARTESIAN_POINT('Ctrl Pts',(-26.7311521296313,-0.591760614150655,
2.51334627463049));
#7190=CARTESIAN_POINT('Ctrl Pts',(-26.7359439235075,-0.585177012577659,
2.51546959688903));
#7191=CARTESIAN_POINT('Ctrl Pts',(-26.7453802030872,-0.57187305643892,2.51968170745714));
#7192=CARTESIAN_POINT('Ctrl Pts',(-26.7500338491731,-0.565138866716563,
2.52177466043333));
#7193=CARTESIAN_POINT('Ctrl Pts',(-26.7637209428383,-0.54480259527845,2.52797323999352));
#7194=CARTESIAN_POINT('Ctrl Pts',(-26.7724790166661,-0.53107397428613,2.53199736377097));
#7195=CARTESIAN_POINT('Ctrl Pts',(-26.7892933503868,-0.503246810054303,
2.53981607542183));
#7196=CARTESIAN_POINT('Ctrl Pts',(-26.7973464004641,-0.489153240022056,
2.54360923524378));
#7197=CARTESIAN_POINT('Ctrl Pts',(-26.8204531754342,-0.446331963437201,
2.55460789831045));
#7198=CARTESIAN_POINT('Ctrl Pts',(-26.8344570585593,-0.417064919965779,
2.56143305219685));
#7199=CARTESIAN_POINT('Ctrl Pts',(-26.8596473785478,-0.357056801425746,
2.57389602618921));
#7200=CARTESIAN_POINT('Ctrl Pts',(-26.8708351093533,-0.326306410018251,
2.5795350016813));
#7201=CARTESIAN_POINT('Ctrl Pts',(-26.8854188856716,-0.279044721282975,
2.58696387685385));
#7202=CARTESIAN_POINT('Ctrl Pts',(-26.889916181885,-0.263080008230857,2.58927006723958));
#7203=CARTESIAN_POINT('Ctrl Pts',(-26.8981455932565,-0.23078565943978,2.59350988787545));
#7204=CARTESIAN_POINT('Ctrl Pts',(-26.9018527777375,-0.214553232694009,
2.5954306174658));
#7205=CARTESIAN_POINT('Ctrl Pts',(-26.9084592496751,-0.181885630631591,
2.59886572989619));
#7206=CARTESIAN_POINT('Ctrl Pts',(-26.9113559512979,-0.165463618176975,
2.60037877253407));
#7207=CARTESIAN_POINT('Ctrl Pts',(-26.9163368119689,-0.13239300581574,2.60298704123573));
#7208=CARTESIAN_POINT('Ctrl Pts',(-26.9184090029522,-0.115817353571131,
2.6040759965005));
#7209=CARTESIAN_POINT('Ctrl Pts',(-26.9233578038635,-0.0661857319676012,
2.60668048407777));
#7210=CARTESIAN_POINT('Ctrl Pts',(-26.9249957317331,-0.0331163807650857,
2.60754764115516));
#7211=CARTESIAN_POINT('Ctrl Pts',(-26.9249997882108,0.0164340525421226,
2.60754980435113));
#7212=CARTESIAN_POINT('Ctrl Pts',(-26.924592211501,0.0329434099001457,2.60733433932482));
#7213=CARTESIAN_POINT('Ctrl Pts',(-26.922958321114,0.0659472086648965,2.60647188023517));
#7214=CARTESIAN_POINT('Ctrl Pts',(-26.9217320306451,0.0824416504222714,
2.60582488664723));
#7215=CARTESIAN_POINT('Ctrl Pts',(-26.9184538736218,0.11541551540594,2.60409958669229));
#7216=CARTESIAN_POINT('Ctrl Pts',(-26.9164009929087,0.131898419449027,2.60302074629033));
#7217=CARTESIAN_POINT('Ctrl Pts',(-26.911460595836,0.164835084256703,2.60043347726538));
#7218=CARTESIAN_POINT('Ctrl Pts',(-26.9085597921968,0.181339379062666,2.59891817499628));
#7219=CARTESIAN_POINT('Ctrl Pts',(-26.9019928975065,0.213907595706393,2.59550331376099));
#7220=CARTESIAN_POINT('Ctrl Pts',(-26.8983166368945,0.230050772994289,2.59359841481876));
#7221=CARTESIAN_POINT('Ctrl Pts',(-26.8902023083891,0.262017358841772,2.58941709788185));
#7222=CARTESIAN_POINT('Ctrl Pts',(-26.8857631894022,0.277848484290424,2.58714012203647));
#7223=CARTESIAN_POINT('Ctrl Pts',(-26.8713173449163,0.324894779397641,2.57977903284149));
#7224=CARTESIAN_POINT('Ctrl Pts',(-26.8601819442124,0.355668892391147,2.57416342317006));
#7225=CARTESIAN_POINT('Ctrl Pts',(-26.8412486366545,0.400939993511194,2.56479183005488));
#7226=CARTESIAN_POINT('Ctrl Pts',(-26.8345590268073,0.415893141702933,2.56150689497222));
#7227=CARTESIAN_POINT('Ctrl Pts',(-26.823967020712,0.438089012396727,2.55635832654132));
#7228=CARTESIAN_POINT('Ctrl Pts',(-26.8203396689083,0.445455430851153,2.55460350724556));
#7229=CARTESIAN_POINT('Ctrl Pts',(-26.8128985600938,0.460108665512343,2.55102277071131));
#7230=CARTESIAN_POINT('Ctrl Pts',(-26.8090795604559,0.467404628169107,2.54919438667112));
#7231=CARTESIAN_POINT('Ctrl Pts',(-26.797394241101,0.489073962305602,2.54363152212406));
#7232=CARTESIAN_POINT('Ctrl Pts',(-26.789289060049,0.503254782620711,2.53981402566018));
#7233=CARTESIAN_POINT('Ctrl Pts',(-26.7724543674525,0.531113894213035,2.53198595664959));
#7234=CARTESIAN_POINT('Ctrl Pts',(-26.7637261115164,0.544790196579881,2.52797594056181));
#7235=CARTESIAN_POINT('Ctrl Pts',(-26.7366204601151,0.585077837829156,2.51569932133656));
#7236=CARTESIAN_POINT('Ctrl Pts',(-26.7173245039422,0.610949544590526,2.50718576295211));
#7237=CARTESIAN_POINT('Ctrl Pts',(-26.6865409768543,0.648314158915958,2.49408419229669));
#7238=CARTESIAN_POINT('Ctrl Pts',(-26.6759726166714,0.660528085389509,2.48966171422195));
#7239=CARTESIAN_POINT('Ctrl Pts',(-26.6542132239272,0.684474388015626,2.48073390605899));
#7240=CARTESIAN_POINT('Ctrl Pts',(-26.6430264626965,0.696202382055636,2.4762302346818));
#7241=CARTESIAN_POINT('Ctrl Pts',(-26.6257563658622,0.713443816566611,2.46942885891313));
#7242=CARTESIAN_POINT('Ctrl Pts',(-26.6199203558455,0.71912933805822,2.46715519418601));
#7243=CARTESIAN_POINT('Ctrl Pts',(-26.6081482145809,0.730321546007037,2.46262131897029));
#7244=CARTESIAN_POINT('Ctrl Pts',(-26.6022012925659,0.735839132509788,2.46035683871519));
#7245=CARTESIAN_POINT('Ctrl Pts',(-26.5841980514885,0.752140229430916,2.45358395979733));
#7246=CARTESIAN_POINT('Ctrl Pts',(-26.5719627057113,0.762688893231257,2.44908952535157));
#7247=CARTESIAN_POINT('Ctrl Pts',(-26.5345850153881,0.793372503429236,2.43572354204093));
#7248=CARTESIAN_POINT('Ctrl Pts',(-26.5087533968938,0.812566724291233,2.42696101356095));
#7249=CARTESIAN_POINT('Ctrl Pts',(-26.4686207796459,0.83948227304429,2.41422655155215));
#7250=CARTESIAN_POINT('Ctrl Pts',(-26.4550114406092,0.848141391767837,2.4100497583254));
#7251=CARTESIAN_POINT('Ctrl Pts',(-26.4273190367366,0.864830292639679,2.40186446327311));
#7252=CARTESIAN_POINT('Ctrl Pts',(-26.4132360104195,0.872860114977211,2.39785591495116));
#7253=CARTESIAN_POINT('Ctrl Pts',(-26.384582055835,0.888281159414966,2.39004076104537));
#7254=CARTESIAN_POINT('Ctrl Pts',(-26.3700168965852,0.895669478070531,2.38623564655444));
#7255=CARTESIAN_POINT('Ctrl Pts',(-26.3477718580352,0.906270310920229,2.38070172959633));
#7256=CARTESIAN_POINT('Ctrl Pts',(-26.3402920246762,0.909722137727452,2.3788867625548));
#7257=CARTESIAN_POINT('Ctrl Pts',(-26.3252941333419,0.916420286651386,2.37534201103856));
#7258=CARTESIAN_POINT('Ctrl Pts',(-26.3177603512233,0.919674724840875,2.37360807070524));
#7259=CARTESIAN_POINT('Ctrl Pts',(-26.2799597723219,0.935450414400031,2.36515131650747));
#7260=CARTESIAN_POINT('Ctrl Pts',(-26.2492303116149,0.946538086235351,2.35904259359383));
#7261=CARTESIAN_POINT('Ctrl Pts',(-26.1868085832625,0.965668578368483,2.34833591063874));
#7262=CARTESIAN_POINT('Ctrl Pts',(-26.1551124003162,0.973715224519582,2.34373600934578));
#7263=CARTESIAN_POINT('Ctrl Pts',(-26.1068141625445,0.983466877886528,2.33810786542034));
#7264=CARTESIAN_POINT('Ctrl Pts',(-26.0905889199931,0.986330406808494,2.33644376922427));
#7265=CARTESIAN_POINT('Ctrl Pts',(-26.0578798138568,0.991267004789931,2.33356356824836));
#7266=CARTESIAN_POINT('Ctrl Pts',(-26.0413987784432,0.993339559141257,2.33234779729884));
#7267=CARTESIAN_POINT('Ctrl Pts',(-26.0164682576784,0.995840021233325,2.33087747927257));
#7268=CARTESIAN_POINT('Ctrl Pts',(-26.0081136505026,0.996572064821657,2.33044626591382));
#7269=CARTESIAN_POINT('Ctrl Pts',(-25.9914405419907,0.997822188899716,2.3297091449783));
#7270=CARTESIAN_POINT('Ctrl Pts',(-25.983108979154,0.99834196239474,2.32940224532968));
#7271=CARTESIAN_POINT('Ctrl Pts',(-25.9581619401288,0.999585267481797,2.32866771122069));
#7272=CARTESIAN_POINT('Ctrl Pts',(-25.9415535530913,0.999997281825182,2.32842370354953));
#7273=CARTESIAN_POINT('Ctrl Pts',(-25.8918801633427,0.999995995609899,2.32842452644233));
#7274=CARTESIAN_POINT('Ctrl Pts',(-25.8588977400795,0.998354960350003,2.32939847806693));
#7275=CARTESIAN_POINT('Ctrl Pts',(-25.809655632564,0.993459342757429,2.3322774437906));
#7276=CARTESIAN_POINT('Ctrl Pts',(-25.7932782734797,0.991421278478362,2.33347323218692));
#7277=CARTESIAN_POINT('Ctrl Pts',(-25.7605969584102,0.986528474355782,2.33632851316856));
#7278=CARTESIAN_POINT('Ctrl Pts',(-25.7442875327586,0.983672349909096,2.33798881805762));
#7279=CARTESIAN_POINT('Ctrl Pts',(-25.7198951962202,0.978772165598707,2.34081761913493));
#7280=CARTESIAN_POINT('Ctrl Pts',(-25.7117696482312,0.977034217384609,2.34181798163729));
#7281=CARTESIAN_POINT('Ctrl Pts',(-25.6955367491711,0.973349801421764,2.34393091101302));
#7282=CARTESIAN_POINT('Ctrl Pts',(-25.6874344702097,0.971403984435815,2.34504307866984));
#7283=CARTESIAN_POINT('Ctrl Pts',(-25.6632988267017,0.96528820198757,2.34852442457186));
#7284=CARTESIAN_POINT('Ctrl Pts',(-25.6473898327442,0.960831588438278,2.35104334024925));
#7285=CARTESIAN_POINT('Ctrl Pts',(-25.6159256353873,0.951177087518203,2.35644596476354));
#7286=CARTESIAN_POINT('Ctrl Pts',(-25.6003698930602,0.945979355455201,2.35932958924631));
#7287=CARTESIAN_POINT('Ctrl Pts',(-25.5696016033233,0.934854907919272,2.36543090574196));
#7288=CARTESIAN_POINT('Ctrl Pts',(-25.5543890761051,0.928928152287264,2.36864862443055));
#7289=CARTESIAN_POINT('Ctrl Pts',(-25.5092559713361,0.910063051819399,2.37875853937475));
#7290=CARTESIAN_POINT('Ctrl Pts',(-25.4798371327009,0.896039907812121,2.38610847112559));
#7291=CARTESIAN_POINT('Ctrl Pts',(-25.4438916664408,0.876696452792296,2.39591178467007));
#7292=CARTESIAN_POINT('Ctrl Pts',(-25.4367422081294,0.872734553740163,2.39790417870507));
#7293=CARTESIAN_POINT('Ctrl Pts',(-25.4225301197978,0.86463029533237,2.40194577660712));
#7294=CARTESIAN_POINT('Ctrl Pts',(-25.415458892085,0.860482058534005,2.40399774819588));
#7295=CARTESIAN_POINT('Ctrl Pts',(-25.3944665440157,0.847818132221257,2.41020698379142));
#7296=CARTESIAN_POINT('Ctrl Pts',(-25.3807469194853,0.839074603637398,2.41442221810216));
#7297=CARTESIAN_POINT('Ctrl Pts',(-25.3538269146123,0.820986612312243,2.42297440207294));
#7298=CARTESIAN_POINT('Ctrl Pts',(-25.3406288513095,0.811643743807886,2.42731061510823));
#7299=CARTESIAN_POINT('Ctrl Pts',(-25.3147440120878,0.792365407430321,2.43607078110781));
#7300=CARTESIAN_POINT('Ctrl Pts',(-25.302057253131,0.782429927595721,2.44049476170448));
#7301=CARTESIAN_POINT('Ctrl Pts',(-25.2771870451046,0.761966360498873,2.44939937123357));
#7302=CARTESIAN_POINT('Ctrl Pts',(-25.2650036031527,0.751438272731137,2.45388002625663));
#7303=CARTESIAN_POINT('Ctrl Pts',(-25.2411363975391,0.729784484637599,2.46286776721369));
#7304=CARTESIAN_POINT('Ctrl Pts',(-25.2294526316117,0.718658795136038,2.46737487908639));
#7305=CARTESIAN_POINT('Ctrl Pts',(-25.2065854499521,0.695799709481914,2.47638573024673));
#7306=CARTESIAN_POINT('Ctrl Pts',(-25.1954025574532,0.684066558646466,2.48088932142673));
#7307=CARTESIAN_POINT('Ctrl Pts',(-25.1790057014816,0.665998774177082,2.48762031005077));
#7308=CARTESIAN_POINT('Ctrl Pts',(-25.1735972102193,0.659890699564589,2.4898624281692));
#7309=CARTESIAN_POINT('Ctrl Pts',(-25.162950610077,0.647566600651522,2.49431653723255));
#7310=CARTESIAN_POINT('Ctrl Pts',(-25.157711714779,0.641350879252783,2.49652867473457));
#7311=CARTESIAN_POINT('Ctrl Pts',(-25.1319370754269,0.609998354556983,2.50750690290623));
#7312=CARTESIAN_POINT('Ctrl Pts',(-25.1126444312025,0.584052119288382,2.51602690308558));
#7313=CARTESIAN_POINT('Ctrl Pts',(-25.0766572872409,0.530427486923958,2.53233703039074));
#7314=CARTESIAN_POINT('Ctrl Pts',(-25.059961236299,0.502749651254307,2.54012821991269));
#7315=CARTESIAN_POINT('Ctrl Pts',(-25.0368800991623,0.459893940418662,2.5511186769858));
#7316=CARTESIAN_POINT('Ctrl Pts',(-25.0295141239499,0.445385200926366,2.55466616380487));
#7317=CARTESIAN_POINT('Ctrl Pts',(-25.0154489582634,0.415908528063232,2.5615030596008));
#7318=CARTESIAN_POINT('Ctrl Pts',(-25.0087494145486,0.40093905147491,2.56479267814122));
#7319=CARTESIAN_POINT('Ctrl Pts',(-24.9992139025481,0.378133256488474,2.56951273362108));
#7320=CARTESIAN_POINT('Ctrl Pts',(-24.9961168386391,0.370460488165633,2.57105248627292));
#7321=CARTESIAN_POINT('Ctrl Pts',(-24.9901160989215,0.355044978918723,2.57404734396978));
#7322=CARTESIAN_POINT('Ctrl Pts',(-24.9872176813169,0.347316938912865,2.57549979202267));
#7323=CARTESIAN_POINT('Ctrl Pts',(-24.978825003649,0.324068265856255,2.57972038676598));
#7324=CARTESIAN_POINT('Ctrl Pts',(-24.9736233181388,0.30846143145007,2.5823566152535));
#7325=CARTESIAN_POINT('Ctrl Pts',(-24.9640114746886,0.277068877280406,2.58725544515496));
#7326=CARTESIAN_POINT('Ctrl Pts',(-24.9595988320509,0.261277274869764,2.58951929498313));
#7327=CARTESIAN_POINT('Ctrl Pts',(-24.9515558748388,0.229503410355285,2.59366439634911));
#7328=CARTESIAN_POINT('Ctrl Pts',(-24.9479255650923,0.213521148150428,2.59554565951957));
#7329=CARTESIAN_POINT('Ctrl Pts',(-24.9414489760593,0.181364697617431,2.59891367071842));
#7330=CARTESIAN_POINT('Ctrl Pts',(-24.9386026892397,0.165190511764198,2.60040043074176));
#7331=CARTESIAN_POINT('Ctrl Pts',(-24.9337017706775,0.13264767434638,2.60296683712999));
#7332=CARTESIAN_POINT('Ctrl Pts',(-24.9316471184334,0.116279028004551,2.60404649646));
#7333=CARTESIAN_POINT('Ctrl Pts',(-24.9283432634801,0.0833433888462451,
2.60578520034254));
#7334=CARTESIAN_POINT('Ctrl Pts',(-24.9270943388138,0.0667755622802239,
2.60644409327794));
#7335=CARTESIAN_POINT('Ctrl Pts',(-24.9258394406481,0.0417735825487931,
2.60710648445228));
#7336=CARTESIAN_POINT('Ctrl Pts',(-24.9255244961035,0.0334015655269924,
2.6072728288538));
#7337=CARTESIAN_POINT('Ctrl Pts',(-24.9251056202904,0.0166741410701568,
2.60749409590418));
#7338=CARTESIAN_POINT('Ctrl Pts',(-24.9250013822027,0.00832706674008074,
2.60754917994844));
#7339=CARTESIAN_POINT('Ctrl Pts',(-24.925001560524,1.55857043960029E-16,
2.60754908509522));
#7340=CARTESIAN_POINT('Ctrl Pts',(-24.7512201965622,1.27647978108407E-15,
-3.00000124311957));
#7341=CARTESIAN_POINT('Ctrl Pts',(-24.7512206151827,0.0224904615946214,
-3.00000102486114));
#7342=CARTESIAN_POINT('Ctrl Pts',(-24.7517085809449,0.0449131097845636,
-2.99974818887592));
#7343=CARTESIAN_POINT('Ctrl Pts',(-24.7536439761057,0.0895752885321371,
-2.99874684907646));
#7344=CARTESIAN_POINT('Ctrl Pts',(-24.7550910425168,0.111823263408203,-2.99799854559508));
#7345=CARTESIAN_POINT('Ctrl Pts',(-24.7608541223483,0.178321019824607,-2.99502561769244));
#7346=CARTESIAN_POINT('Ctrl Pts',(-24.7665915611397,0.222335311776172,-2.99207181620779));
#7347=CARTESIAN_POINT('Ctrl Pts',(-24.7780288192454,0.287837360410405,-2.98624162780084));
#7348=CARTESIAN_POINT('Ctrl Pts',(-24.7823197307722,0.309606561385101,-2.98406194825969));
#7349=CARTESIAN_POINT('Ctrl Pts',(-24.7894679779365,0.34210979841364,-2.98045092915735));
#7350=CARTESIAN_POINT('Ctrl Pts',(-24.7919724393738,0.352930055186471,-2.97918882741414));
#7351=CARTESIAN_POINT('Ctrl Pts',(-24.7972214032702,0.374523340751588,-2.97655141398561));
#7352=CARTESIAN_POINT('Ctrl Pts',(-24.7999681707864,0.38530289681448,-2.97517498996412));
#7353=CARTESIAN_POINT('Ctrl Pts',(-24.8085247289755,0.417396325006842,-2.97090101111402));
#7354=CARTESIAN_POINT('Ctrl Pts',(-24.8146611612218,0.438519664833834,-2.96785340267611));
#7355=CARTESIAN_POINT('Ctrl Pts',(-24.827780795185,0.480245605735748,-2.96138777142348));
#7356=CARTESIAN_POINT('Ctrl Pts',(-24.8347634091537,0.500846985261602,-2.95797002138279));
#7357=CARTESIAN_POINT('Ctrl Pts',(-24.8569585745012,0.56188530630259,-2.94720211826449));
#7358=CARTESIAN_POINT('Ctrl Pts',(-24.8734157851973,0.601558415893423,-2.93933707448591));
#7359=CARTESIAN_POINT('Ctrl Pts',(-24.9005699650057,0.659577946472717,-2.92666307786021));
#7360=CARTESIAN_POINT('Ctrl Pts',(-24.9100343005407,0.678670330222986,-2.92229185258577));
#7361=CARTESIAN_POINT('Ctrl Pts',(-24.9297925040438,0.716356052195618,-2.91328291034591));
#7362=CARTESIAN_POINT('Ctrl Pts',(-24.9400941970776,0.734962854491031,-2.90864166879987));
#7363=CARTESIAN_POINT('Ctrl Pts',(-24.9615143509208,0.771630108002674,-2.8991297911222));
#7364=CARTESIAN_POINT('Ctrl Pts',(-24.9725542617936,0.789558390564705,-2.89429401664935));
#7365=CARTESIAN_POINT('Ctrl Pts',(-24.9953081681755,0.824675412874893,-2.88448450367961));
#7366=CARTESIAN_POINT('Ctrl Pts',(-25.0070176561689,0.841856330313487,-2.87951274183947));
#7367=CARTESIAN_POINT('Ctrl Pts',(-25.0431332882325,0.892293349065714,-2.86444629839691));
#7368=CARTESIAN_POINT('Ctrl Pts',(-25.0685240643679,0.924446248154153,-2.85419987571196));
#7369=CARTESIAN_POINT('Ctrl Pts',(-25.1085917532924,0.970519332950315,-2.83872559859403));
#7370=CARTESIAN_POINT('Ctrl Pts',(-25.1222785365167,0.985516952511361,-2.83355000263622));
#7371=CARTESIAN_POINT('Ctrl Pts',(-25.1503245087481,1.01479156009321,-2.82319808714425));
#7372=CARTESIAN_POINT('Ctrl Pts',(-25.1646905450052,1.02907433729269,-2.81801945772865));
#7373=CARTESIAN_POINT('Ctrl Pts',(-25.1940839460452,1.05688985201169,-2.80770598732435));
#7374=CARTESIAN_POINT('Ctrl Pts',(-25.2091788350748,1.07047868451994,-2.80254912945966));
#7375=CARTESIAN_POINT('Ctrl Pts',(-25.2397857985023,1.09666875082296,-2.79240445901191));
#7376=CARTESIAN_POINT('Ctrl Pts',(-25.255320223101,1.10929658351523,-2.78740768552752));
#7377=CARTESIAN_POINT('Ctrl Pts',(-25.2868469170525,1.13362940492585,-2.77760057560581));
#7378=CARTESIAN_POINT('Ctrl Pts',(-25.302839623016,1.1453353693059,-2.77278994432858));
#7379=CARTESIAN_POINT('Ctrl Pts',(-25.3352860491081,1.16783592991972,-2.76338858760641));
#7380=CARTESIAN_POINT('Ctrl Pts',(-25.3517397751987,1.17863049873126,-2.75879782839759));
#7381=CARTESIAN_POINT('Ctrl Pts',(-25.4018014264425,1.20964993058027,-2.74540766718038));
#7382=CARTESIAN_POINT('Ctrl Pts',(-25.4361157965431,1.22851722530087,-2.7369879943305));
#7383=CARTESIAN_POINT('Ctrl Pts',(-25.4890319606085,1.25402748115623,-2.72534609489846));
#7384=CARTESIAN_POINT('Ctrl Pts',(-25.5069294362475,1.26207118462113,-2.72162720547796));
#7385=CARTESIAN_POINT('Ctrl Pts',(-25.5341341065867,1.2734147976899,-2.71632858891394));
#7386=CARTESIAN_POINT('Ctrl Pts',(-25.5432727036745,1.27707929627405,-2.71460725980808));
#7387=CARTESIAN_POINT('Ctrl Pts',(-25.5616696134459,1.28416319515222,-2.71126336921716));
#7388=CARTESIAN_POINT('Ctrl Pts',(-25.5709426986925,1.28758734347614,-2.70963852456332));
#7389=CARTESIAN_POINT('Ctrl Pts',(-25.5987920948568,1.29743244195315,-2.70494558321287));
#7390=CARTESIAN_POINT('Ctrl Pts',(-25.617433882299,1.30344363716718,-2.70205116137012));
#7391=CARTESIAN_POINT('Ctrl Pts',(-25.6548879621502,1.31438372733535,-2.69674641877481));
#7392=CARTESIAN_POINT('Ctrl Pts',(-25.6736968490448,1.31931173160549,-2.69433651551851));
#7393=CARTESIAN_POINT('Ctrl Pts',(-25.7303690237763,1.33248274213306,-2.68786059982171));
#7394=CARTESIAN_POINT('Ctrl Pts',(-25.7684773832559,1.33911643529057,-2.6845486252675));
#7395=CARTESIAN_POINT('Ctrl Pts',(-25.8261391213393,1.34582410918547,-2.68118864483475));
#7396=CARTESIAN_POINT('Ctrl Pts',(-25.8454430068625,1.34751862690546,-2.68033657178925));
#7397=CARTESIAN_POINT('Ctrl Pts',(-25.8842203794928,1.34980853567156,-2.67918411053142));
#7398=CARTESIAN_POINT('Ctrl Pts',(-25.9037051371427,1.35040321450497,-2.67888411665588));
#7399=CARTESIAN_POINT('Ctrl Pts',(-25.9428031440834,1.35047173299046,-2.67884957398268));
#7400=CARTESIAN_POINT('Ctrl Pts',(-25.9625262788924,1.34993763378489,-2.67911903945912));
#7401=CARTESIAN_POINT('Ctrl Pts',(-26.001675179068,1.34774256849849,-2.68022395142751));
#7402=CARTESIAN_POINT('Ctrl Pts',(-26.0211401464231,1.34608753889996,-2.68105638390197));
#7403=CARTESIAN_POINT('Ctrl Pts',(-26.0598521561959,1.34168374443806,-2.68326288816888));
#7404=CARTESIAN_POINT('Ctrl Pts',(-26.0790999491839,1.33893558390627,-2.68463664029073));
#7405=CARTESIAN_POINT('Ctrl Pts',(-26.1173832731121,1.33236285214625,-2.68790468740719));
#7406=CARTESIAN_POINT('Ctrl Pts',(-26.1364187960914,1.32853823376571,-2.68979898789909));
#7407=CARTESIAN_POINT('Ctrl Pts',(-26.1932112333693,1.31546132541519,-2.69623160867151));
#7408=CARTESIAN_POINT('Ctrl Pts',(-26.230658868257,1.30460568802835,-2.70152164206104));
#7409=CARTESIAN_POINT('Ctrl Pts',(-26.2769394358952,1.28835579481113,-2.70927322407079));
#7410=CARTESIAN_POINT('Ctrl Pts',(-26.2861736873588,1.28496804550344,-2.71088197061785));
#7411=CARTESIAN_POINT('Ctrl Pts',(-26.3045801226384,1.27792632816734,-2.71420859259991));
#7412=CARTESIAN_POINT('Ctrl Pts',(-26.3137696612827,1.2742643583807,-2.71593014837301));
#7413=CARTESIAN_POINT('Ctrl Pts',(-26.3411343470425,1.26292005406289,-2.72123342520569));
#7414=CARTESIAN_POINT('Ctrl Pts',(-26.3591086288947,1.25488236548528,-2.72495256846717));
#7415=CARTESIAN_POINT('Ctrl Pts',(-26.3945730991822,1.23786441433936,-2.73272536195925));
#7416=CARTESIAN_POINT('Ctrl Pts',(-26.4120574252086,1.22888679609907,-2.73677778918298));
#7417=CARTESIAN_POINT('Ctrl Pts',(-26.4465443911629,1.21000870437875,-2.74517655409932));
#7418=CARTESIAN_POINT('Ctrl Pts',(-26.4635470144595,1.20010820517652,-2.74952291627503));
#7419=CARTESIAN_POINT('Ctrl Pts',(-26.4970806133762,1.1793905896332,-2.75847308374743));
#7420=CARTESIAN_POINT('Ctrl Pts',(-26.5136115807888,1.16857346524795,-2.76307691198199));
#7421=CARTESIAN_POINT('Ctrl Pts',(-26.546208083381,1.14602103189425,-2.77250675337683));
#7422=CARTESIAN_POINT('Ctrl Pts',(-26.5622736983626,1.1342856634169,-2.77733281570969));
#7423=CARTESIAN_POINT('Ctrl Pts',(-26.5939416429695,1.10988763337468,-2.7871725670388));
#7424=CARTESIAN_POINT('Ctrl Pts',(-26.609547564207,1.09722193187052,-2.79218745199254));
#7425=CARTESIAN_POINT('Ctrl Pts',(-26.6402813438902,1.0709572172429,-2.8023664037371));
#7426=CARTESIAN_POINT('Ctrl Pts',(-26.655295080658,1.05745634546246,-2.80749236059604));
#7427=CARTESIAN_POINT('Ctrl Pts',(-26.6846548548111,1.02971401041124,-2.81778570291711));
#7428=CARTESIAN_POINT('Ctrl Pts',(-26.698997953854,1.01547501212972,-2.82295214467571));
#7429=CARTESIAN_POINT('Ctrl Pts',(-26.7270253212179,0.986266221033504,-2.83328911051858));
#7430=CARTESIAN_POINT('Ctrl Pts',(-26.7407095447861,0.971296396677911,-2.83845969056953));
#7431=CARTESIAN_POINT('Ctrl Pts',(-26.7807872610901,0.925288863725479,-2.85392633511737));
#7432=CARTESIAN_POINT('Ctrl Pts',(-26.8062107356642,0.893151941339911,-2.864178670324));
#7433=CARTESIAN_POINT('Ctrl Pts',(-26.8423947744529,0.84270457925161,-2.87926472137709));
#7434=CARTESIAN_POINT('Ctrl Pts',(-26.8541358893937,0.825504953419084,-2.88424727122285));
#7435=CARTESIAN_POINT('Ctrl Pts',(-26.8712465648999,0.799139107619223,-2.89162033090013));
#7436=CARTESIAN_POINT('Ctrl Pts',(-26.8768710845513,0.79024832752982,-2.89406322620423));
#7437=CARTESIAN_POINT('Ctrl Pts',(-26.8879472162261,0.772282090199624,-2.89890928529195));
#7438=CARTESIAN_POINT('Ctrl Pts',(-26.8934095805383,0.763187949365322,-2.9013172405501));
#7439=CARTESIAN_POINT('Ctrl Pts',(-26.9094752397211,0.735724969537463,-2.90844874441802));
#7440=CARTESIAN_POINT('Ctrl Pts',(-26.9197553059395,0.717185246436085,-2.91307852354811));
#7441=CARTESIAN_POINT('Ctrl Pts',(-26.939491662068,0.679606241243716,-2.92207399934037));
#7442=CARTESIAN_POINT('Ctrl Pts',(-26.9489441843561,0.660573675186059,-2.92643805302077));
#7443=CARTESIAN_POINT('Ctrl Pts',(-26.9760664924628,0.602745972669876,-2.93909208245403));
#7444=CARTESIAN_POINT('Ctrl Pts',(-26.9925039932974,0.563222492320482,-2.94694446393472));
#7445=CARTESIAN_POINT('Ctrl Pts',(-27.0220719282814,0.482184935663522,-2.96128319208414));
#7446=CARTESIAN_POINT('Ctrl Pts',(-27.0352038812473,0.440658278132658,-2.96777086803717));
#7447=CARTESIAN_POINT('Ctrl Pts',(-27.0523220500515,0.376834051179658,-2.97631783456127));
#7448=CARTESIAN_POINT('Ctrl Pts',(-27.0576008937577,0.355274612711088,-2.97897112077082));
#7449=CARTESIAN_POINT('Ctrl Pts',(-27.0672604256937,0.311662928430509,-2.98384906046174));
#7450=CARTESIAN_POINT('Ctrl Pts',(-27.0716118507556,0.28974195783202,-2.98605887165636));
#7451=CARTESIAN_POINT('Ctrl Pts',(-27.0793664061891,0.245626216202852,-2.99001098961276));
#7452=CARTESIAN_POINT('Ctrl Pts',(-27.0827665013565,0.223449220869779,-2.99175175446374));
#7453=CARTESIAN_POINT('Ctrl Pts',(-27.0886129441394,0.178789236716058,-2.99475258363014));
#7454=CARTESIAN_POINT('Ctrl Pts',(-27.0910452438611,0.156404759559941,-2.99600543335325));
#7455=CARTESIAN_POINT('Ctrl Pts',(-27.0968540554839,0.0893800728363459,
-2.99900191231137));
#7456=CARTESIAN_POINT('Ctrl Pts',(-27.0987766251388,0.044721791781682,-2.99999958185766));
#7457=CARTESIAN_POINT('Ctrl Pts',(-27.0987813865579,-0.0221932547862428,
-3.00000207062791));
#7458=CARTESIAN_POINT('Ctrl Pts',(-27.098302980501,-0.0444882044529787,
-2.99975417679133));
#7459=CARTESIAN_POINT('Ctrl Pts',(-27.0963851499708,-0.0890579606384743,
-2.99876191230976));
#7460=CARTESIAN_POINT('Ctrl Pts',(-27.0949457527391,-0.111332767632209,
-2.99801754221172));
#7461=CARTESIAN_POINT('Ctrl Pts',(-27.091097912228,-0.155862099946069,-2.99603257401337));
#7462=CARTESIAN_POINT('Ctrl Pts',(-27.0886882785475,-0.178121325914285,
-2.99479136150237));
#7463=CARTESIAN_POINT('Ctrl Pts',(-27.0828893311938,-0.222600421497835,
-2.99181469259339));
#7464=CARTESIAN_POINT('Ctrl Pts',(-27.0794844211542,-0.244888534479487,
-2.99007132802239));
#7465=CARTESIAN_POINT('Ctrl Pts',(-27.0717763207677,-0.288870061738491,
-2.98614250919086));
#7466=CARTESIAN_POINT('Ctrl Pts',(-27.0674611935747,-0.310670506014757,
-2.98395091125391));
#7467=CARTESIAN_POINT('Ctrl Pts',(-27.0579367437935,-0.353839565051261,
-2.9791402804281));
#7468=CARTESIAN_POINT('Ctrl Pts',(-27.0527261874502,-0.37521860103612,-2.97652060572815));
#7469=CARTESIAN_POINT('Ctrl Pts',(-27.0357699204893,-0.438751951157215,
-2.96805162738344));
#7470=CARTESIAN_POINT('Ctrl Pts',(-27.022699391642,-0.480310643319726,-2.96159083395379));
#7471=CARTESIAN_POINT('Ctrl Pts',(-27.0004758229384,-0.541446694763503,
-2.95080875849622));
#7472=CARTESIAN_POINT('Ctrl Pts',(-26.992623681753,-0.561640072316635,-2.94702942050088));
#7473=CARTESIAN_POINT('Ctrl Pts',(-26.9801909795193,-0.591614335345471,
-2.94110596088858));
#7474=CARTESIAN_POINT('Ctrl Pts',(-26.9759332605878,-0.601562265182988,
-2.9390870305072));
#7475=CARTESIAN_POINT('Ctrl Pts',(-26.9671990237161,-0.621350626541995,
-2.93496737112459));
#7476=CARTESIAN_POINT('Ctrl Pts',(-26.9627163520765,-0.631203409825244,
-2.93286380405279));
#7477=CARTESIAN_POINT('Ctrl Pts',(-26.9490003388169,-0.660466615132212,
-2.92646369421333));
#7478=CARTESIAN_POINT('Ctrl Pts',(-26.9394866261483,-0.679617007741934,
-2.92207164107701));
#7479=CARTESIAN_POINT('Ctrl Pts',(-26.9197263731453,-0.717239156030648,
-2.91306539958487));
#7480=CARTESIAN_POINT('Ctrl Pts',(-26.9094813066202,-0.735708225799579,
-2.9084518514383));
#7481=CARTESIAN_POINT('Ctrl Pts',(-26.8776651907974,-0.790114397662374,
-2.8943275255928));
#7482=CARTESIAN_POINT('Ctrl Pts',(-26.855015951808,-0.825052668578734,-2.88453262436396));
#7483=CARTESIAN_POINT('Ctrl Pts',(-26.8188828130475,-0.875511458559026,
-2.86945918682943));
#7484=CARTESIAN_POINT('Ctrl Pts',(-26.806477865951,-0.892005672721584,-2.86437109863275));
#7485=CARTESIAN_POINT('Ctrl Pts',(-26.7809370903558,-0.924343794681306,
-2.85409960048902));
#7486=CARTESIAN_POINT('Ctrl Pts',(-26.7678062754663,-0.940181784684746,
-2.84891809889913));
#7487=CARTESIAN_POINT('Ctrl Pts',(-26.747534952965,-0.963465362975884,-2.8410930742898));
#7488=CARTESIAN_POINT('Ctrl Pts',(-26.7406847515848,-0.971143336910778,
-2.8384772090519));
#7489=CARTESIAN_POINT('Ctrl Pts',(-26.726866828362,-0.986257778221383,-2.8332609577602));
#7490=CARTESIAN_POINT('Ctrl Pts',(-26.7198864405152,-0.993708965489595,
-2.83065565931378));
#7491=CARTESIAN_POINT('Ctrl Pts',(-26.6987545667654,-1.01572267126074,-2.82286342050641));
#7492=CARTESIAN_POINT('Ctrl Pts',(-26.6843929425923,-1.02996804274084,-2.81769254606288));
#7493=CARTESIAN_POINT('Ctrl Pts',(-26.6405196961263,-1.07140451601385,-2.80231490014363));
#7494=CARTESIAN_POINT('Ctrl Pts',(-26.6101990167324,-1.09732522138671,-2.79223355729095));
#7495=CARTESIAN_POINT('Ctrl Pts',(-26.5630920876351,-1.13367314163992,-2.77758248050925));
#7496=CARTESIAN_POINT('Ctrl Pts',(-26.5471176954077,-1.14536678978724,-2.77277705423988));
#7497=CARTESIAN_POINT('Ctrl Pts',(-26.5146128603087,-1.1679042027731,-2.76335982199195));
#7498=CARTESIAN_POINT('Ctrl Pts',(-26.4980824626504,-1.17874802188457,-2.75874796251914));
#7499=CARTESIAN_POINT('Ctrl Pts',(-26.4644489769846,-1.19957326674857,-2.74975657993441));
#7500=CARTESIAN_POINT('Ctrl Pts',(-26.4473526605441,-1.20955077156384,-2.74537877233406));
#7501=CARTESIAN_POINT('Ctrl Pts',(-26.4212418428209,-1.22386659438306,-2.73901196687351));
#7502=CARTESIAN_POINT('Ctrl Pts',(-26.4124621517901,-1.22852809048201,-2.73692383614116));
#7503=CARTESIAN_POINT('Ctrl Pts',(-26.3948579023758,-1.23757356026447,-2.73284557774275));
#7504=CARTESIAN_POINT('Ctrl Pts',(-26.3860148872853,-1.24196849424177,-2.73085066873683));
#7505=CARTESIAN_POINT('Ctrl Pts',(-26.341645261955,-1.26327266721301,-2.72112112107027));
#7506=CARTESIAN_POINT('Ctrl Pts',(-26.3055755853367,-1.27824593843012,-2.71409299783002));
#7507=CARTESIAN_POINT('Ctrl Pts',(-26.2323061069552,-1.30408058177654,-2.70177489330742));
#7508=CARTESIAN_POINT('Ctrl Pts',(-26.1951017095151,-1.314947120491,-2.69648267860914));
#7509=CARTESIAN_POINT('Ctrl Pts',(-26.1384101250037,-1.32811617463851,-2.69000746444321));
#7510=CARTESIAN_POINT('Ctrl Pts',(-26.1193652332726,-1.33198320784822,-2.68809291154563));
#7511=CARTESIAN_POINT('Ctrl Pts',(-26.0809718851876,-1.33864980310861,-2.68477922262698));
#7512=CARTESIAN_POINT('Ctrl Pts',(-26.0616267484912,-1.34144867007466,-2.68338047067986));
#7513=CARTESIAN_POINT('Ctrl Pts',(-26.032363761062,-1.344825402147,-2.68168886075705));
#7514=CARTESIAN_POINT('Ctrl Pts',(-26.0225572765905,-1.34581398544559,-2.6811927471385));
#7515=CARTESIAN_POINT('Ctrl Pts',(-26.0029866880182,-1.3475022070275,-2.68034468497322));
#7516=CARTESIAN_POINT('Ctrl Pts',(-25.9932072525691,-1.34820413161833,-2.67999159504196));
#7517=CARTESIAN_POINT('Ctrl Pts',(-25.9639248763077,-1.34988314454028,-2.6791465090366));
#7518=CARTESIAN_POINT('Ctrl Pts',(-25.944430256616,-1.35043954651562,-2.67886577671176));
#7519=CARTESIAN_POINT('Ctrl Pts',(-25.8861245439706,-1.35043780955491,-2.67886672345498));
#7520=CARTESIAN_POINT('Ctrl Pts',(-25.8474103812661,-1.34822168461924,-2.67998726078285));
#7521=CARTESIAN_POINT('Ctrl Pts',(-25.7896108997839,-1.34161043104657,-2.68329952853648));
#7522=CARTESIAN_POINT('Ctrl Pts',(-25.77038745646,-1.33885814096474,-2.68467529043326));
#7523=CARTESIAN_POINT('Ctrl Pts',(-25.7320267290187,-1.33225068682403,-2.68796030874541));
#7524=CARTESIAN_POINT('Ctrl Pts',(-25.7128830247106,-1.32839365293775,-2.68987049972103));
#7525=CARTESIAN_POINT('Ctrl Pts',(-25.684251748041,-1.3217762322719,-2.69312505274073));
#7526=CARTESIAN_POINT('Ctrl Pts',(-25.6747141290368,-1.31942923189442,-2.69427597594583));
#7527=CARTESIAN_POINT('Ctrl Pts',(-25.6556602502347,-1.31445363734785,-2.69670691417442));
#7528=CARTESIAN_POINT('Ctrl Pts',(-25.6461499439872,-1.31182592199725,-2.69798646989668));
#7529=CARTESIAN_POINT('Ctrl Pts',(-25.6178199688841,-1.30356690507149,-2.70199177974631));
#7530=CARTESIAN_POINT('Ctrl Pts',(-25.5991462839436,-1.29754850153217,-2.70488980770929));
#7531=CARTESIAN_POINT('Ctrl Pts',(-25.5622141869212,-1.28451064624858,-2.71110556040654));
#7532=CARTESIAN_POINT('Ctrl Pts',(-25.5439551422566,-1.27749140423904,-2.7144231880909));
#7533=CARTESIAN_POINT('Ctrl Pts',(-25.5078398888184,-1.26246846951839,-2.72144279020549));
#7534=CARTESIAN_POINT('Ctrl Pts',(-25.4899837037464,-1.25446472257529,-2.72514479532609));
#7535=CARTESIAN_POINT('Ctrl Pts',(-25.4370072942282,-1.22898847560419,-2.7367763145851));
#7536=CARTESIAN_POINT('Ctrl Pts',(-25.4024760017175,-1.21005101589909,-2.74523245622064));
#7537=CARTESIAN_POINT('Ctrl Pts',(-25.3602838735484,-1.18392877826527,-2.75651122868635));
#7538=CARTESIAN_POINT('Ctrl Pts',(-25.3518919706823,-1.1785784585637,-2.75880349026456));
#7539=CARTESIAN_POINT('Ctrl Pts',(-25.3352100824015,-1.16763411776592,-2.76345337348231));
#7540=CARTESIAN_POINT('Ctrl Pts',(-25.3269100051743,-1.16203215951807,-2.76581417940247));
#7541=CARTESIAN_POINT('Ctrl Pts',(-25.3022695725318,-1.1449302461251,-2.77295794310451));
#7542=CARTESIAN_POINT('Ctrl Pts',(-25.2861657292169,-1.1331226072542,-2.77780759607732));
#7543=CARTESIAN_POINT('Ctrl Pts',(-25.2545675218788,-1.10869580205534,-2.78764693628012));
#7544=CARTESIAN_POINT('Ctrl Pts',(-25.2390758775543,-1.09607878865392,-2.7926357760188));
#7545=CARTESIAN_POINT('Ctrl Pts',(-25.208692728647,-1.07004449005285,-2.80271440082356));
#7546=CARTESIAN_POINT('Ctrl Pts',(-25.193801243974,-1.05662718870003,-2.80780421768085));
#7547=CARTESIAN_POINT('Ctrl Pts',(-25.1646090505302,-1.02899230331322,-2.81804902565378));
#7548=CARTESIAN_POINT('Ctrl Pts',(-25.150308350114,-1.0147747185966,-2.82320404678685));
#7549=CARTESIAN_POINT('Ctrl Pts',(-25.1222934624824,-0.985532507337774,
-2.83354449797841));
#7550=CARTESIAN_POINT('Ctrl Pts',(-25.1085792726074,-0.970507895413089,
-2.83872995787953));
#7551=CARTESIAN_POINT('Ctrl Pts',(-25.0817381947277,-0.939637998238792,
-2.84909699750195));
#7552=CARTESIAN_POINT('Ctrl Pts',(-25.0686119208846,-0.923793044275975,
-2.85427840682449));
#7553=CARTESIAN_POINT('Ctrl Pts',(-25.0493655924709,-0.899393527288515,
-2.86202245059147));
#7554=CARTESIAN_POINT('Ctrl Pts',(-25.0430172047533,-0.891144919357547,
-2.86460202126226));
#7555=CARTESIAN_POINT('Ctrl Pts',(-25.0305204210295,-0.874501923571611,
-2.86972650110557));
#7556=CARTESIAN_POINT('Ctrl Pts',(-25.02437110194,-0.866107944767961,-2.87227157889308));
#7557=CARTESIAN_POINT('Ctrl Pts',(-24.9941173036171,-0.823768140450459,
-2.88490209785398));
#7558=CARTESIAN_POINT('Ctrl Pts',(-24.971471952131,-0.788729223015765,-2.89470441040781));
#7559=CARTESIAN_POINT('Ctrl Pts',(-24.9292309034491,-0.716312201964237,
-2.91346931208067));
#7560=CARTESIAN_POINT('Ctrl Pts',(-24.9096333854723,-0.678934856512817,
-2.92243312349527));
#7561=CARTESIAN_POINT('Ctrl Pts',(-24.882541170584,-0.621060652496466,-2.93507771188247));
#7562=CARTESIAN_POINT('Ctrl Pts',(-24.8738951241541,-0.601467423657379,
-2.93915911726366));
#7563=CARTESIAN_POINT('Ctrl Pts',(-24.8573856909762,-0.561660850722057,
-2.94702500788258));
#7564=CARTESIAN_POINT('Ctrl Pts',(-24.8495218895994,-0.541445422596667,
-2.95080973422482));
#7565=CARTESIAN_POINT('Ctrl Pts',(-24.8383292807319,-0.510647491444323,
-2.95624018705409));
#7566=CARTESIAN_POINT('Ctrl Pts',(-24.8346940039926,-0.500285853504755,
-2.95801168194031));
#7567=CARTESIAN_POINT('Ctrl Pts',(-24.8276504459147,-0.479468083601724,
-2.96145728412087));
#7568=CARTESIAN_POINT('Ctrl Pts',(-24.8242483365591,-0.469031804392169,
-2.96312833452968));
#7569=CARTESIAN_POINT('Ctrl Pts',(-24.8143971656437,-0.437635791555516,
-2.96798415471264));
#7570=CARTESIAN_POINT('Ctrl Pts',(-24.8082915227193,-0.416559647886908,
-2.97101715178475));
#7571=CARTESIAN_POINT('Ctrl Pts',(-24.7970093173975,-0.374165786036183,
-2.97665328568467));
#7572=CARTESIAN_POINT('Ctrl Pts',(-24.7918298385069,-0.352840123671072,
-2.97925785882102));
#7573=CARTESIAN_POINT('Ctrl Pts',(-24.782389163039,-0.309931323851523,-2.98402682340998));
#7574=CARTESIAN_POINT('Ctrl Pts',(-24.7781279721287,-0.288348186260508,
-2.98619122824603));
#7575=CARTESIAN_POINT('Ctrl Pts',(-24.7705258708633,-0.244922725747239,
-2.99006614582328));
#7576=CARTESIAN_POINT('Ctrl Pts',(-24.7671849516661,-0.223080406167035,
-2.99177667236476));
#7577=CARTESIAN_POINT('Ctrl Pts',(-24.7614323434624,-0.17913315210593,-2.99472933868235));
#7578=CARTESIAN_POINT('Ctrl Pts',(-24.7590206303916,-0.157028224677867,
-2.99597149337493));
#7579=CARTESIAN_POINT('Ctrl Pts',(-24.7551426261223,-0.11255051417061,-2.99797188287434));
#7580=CARTESIAN_POINT('Ctrl Pts',(-24.7536766612853,-0.0901766051585172,
-2.99872994324477));
#7581=CARTESIAN_POINT('Ctrl Pts',(-24.7522036848644,-0.0564128512141614,
-2.99949202836052));
#7582=CARTESIAN_POINT('Ctrl Pts',(-24.7518340087419,-0.0451069176116392,
-2.9996834086165));
#7583=CARTESIAN_POINT('Ctrl Pts',(-24.751342340005,-0.0225174807117986,
-2.99993797771742));
#7584=CARTESIAN_POINT('Ctrl Pts',(-24.751219987252,-0.0112452307973086,
-3.00000135224878));
#7585=CARTESIAN_POINT('Ctrl Pts',(-24.7512201965622,1.27647978108407E-15,
-3.00000124311957));
#7586=CARTESIAN_POINT('Ctrl Pts',(-24.9250015605239,9.19874578470569E-16,
-2.60754908509523));
#7587=CARTESIAN_POINT('Ctrl Pts',(-24.9250019171665,0.0166541334801639,
-2.60754889538879));
#7588=CARTESIAN_POINT('Ctrl Pts',(-24.9254176382407,0.0332580512905832,
-2.60732913473254));
#7589=CARTESIAN_POINT('Ctrl Pts',(-24.9270664927659,0.0663302887433929,
-2.60645878753387));
#7590=CARTESIAN_POINT('Ctrl Pts',(-24.9282993169708,0.0828048613803127,
-2.60580837511734));
#7591=CARTESIAN_POINT('Ctrl Pts',(-24.9332091568075,0.13204629231987,-2.60322435771041));
#7592=CARTESIAN_POINT('Ctrl Pts',(-24.9380971518304,0.164638771132329,-2.60065696465499));
#7593=CARTESIAN_POINT('Ctrl Pts',(-24.9478410920693,0.213142882820904,-2.59558946593898));
#7594=CARTESIAN_POINT('Ctrl Pts',(-24.9514967222119,0.229262924518064,-2.59369492625984));
#7595=CARTESIAN_POINT('Ctrl Pts',(-24.957586651506,0.253331494462504,-2.59055629104136));
#7596=CARTESIAN_POINT('Ctrl Pts',(-24.9597203204629,0.261343868943604,-2.58945929408072));
#7597=CARTESIAN_POINT('Ctrl Pts',(-24.9641921606581,0.277333645699331,-2.58716690003976));
#7598=CARTESIAN_POINT('Ctrl Pts',(-24.9665322616052,0.28531588140159,-2.58597053613621));
#7599=CARTESIAN_POINT('Ctrl Pts',(-24.9738219975603,0.309080988873586,-2.58225566779539));
#7600=CARTESIAN_POINT('Ctrl Pts',(-24.9790499139481,0.32472277192427,-2.57960673936175));
#7601=CARTESIAN_POINT('Ctrl Pts',(-24.9902271496198,0.355620732215228,-2.57398692473799));
#7602=CARTESIAN_POINT('Ctrl Pts',(-24.9961759681728,0.37087600490021,-2.57101627563854));
#7603=CARTESIAN_POINT('Ctrl Pts',(-25.015085077571,0.416074736889802,-2.5616570008748));
#7604=CARTESIAN_POINT('Ctrl Pts',(-25.0291057524579,0.445452580460475,-2.55482084113839));
#7605=CARTESIAN_POINT('Ctrl Pts',(-25.0522396804357,0.48841590527102,-2.54380482293415));
#7606=CARTESIAN_POINT('Ctrl Pts',(-25.060302794776,0.502553770162824,-2.54000542968693));
#7607=CARTESIAN_POINT('Ctrl Pts',(-25.0771357413066,0.530459957917388,-2.53217501323324));
#7608=CARTESIAN_POINT('Ctrl Pts',(-25.0859122400396,0.544238250893843,-2.5281409265225));
#7609=CARTESIAN_POINT('Ctrl Pts',(-25.1041610805409,0.571390265168163,-2.51987336730303));
#7610=CARTESIAN_POINT('Ctrl Pts',(-25.113566501909,0.5846661158911,-2.51567019594392));
#7611=CARTESIAN_POINT('Ctrl Pts',(-25.1329516291768,0.610670187636857,-2.50714393728714));
#7612=CARTESIAN_POINT('Ctrl Pts',(-25.1429274949106,0.62339261625794,-2.50282256806535));
#7613=CARTESIAN_POINT('Ctrl Pts',(-25.1736961072169,0.660741109040548,-2.48972707655348));
#7614=CARTESIAN_POINT('Ctrl Pts',(-25.195327708338,0.684550254569154,-2.48082106354485));
#7615=CARTESIAN_POINT('Ctrl Pts',(-25.2294632644966,0.718667264605287,-2.46737109007097));
#7616=CARTESIAN_POINT('Ctrl Pts',(-25.2411236814041,0.729772966325552,-2.46287255176687));
#7617=CARTESIAN_POINT('Ctrl Pts',(-25.2650173694561,0.75145074381943,-2.45387484623858));
#7618=CARTESIAN_POINT('Ctrl Pts',(-25.2772564740961,0.762027106466311,-2.44937367130548));
#7619=CARTESIAN_POINT('Ctrl Pts',(-25.3022981003744,0.782624429155002,-2.44040938158116));
#7620=CARTESIAN_POINT('Ctrl Pts',(-25.3151581491073,0.792686927403694,-2.43592713010271));
#7621=CARTESIAN_POINT('Ctrl Pts',(-25.3412336664868,0.812080609394974,-2.42710955837505));
#7622=CARTESIAN_POINT('Ctrl Pts',(-25.3544681763255,0.821431489558632,-2.42276644946543));
#7623=CARTESIAN_POINT('Ctrl Pts',(-25.3813272555676,0.839449886111474,-2.41424227949637));
#7624=CARTESIAN_POINT('Ctrl Pts',(-25.3949521969405,0.848118124975925,-2.41006096216709));
#7625=CARTESIAN_POINT('Ctrl Pts',(-25.4225948394221,0.864779736753664,-2.40188946584664));
#7626=CARTESIAN_POINT('Ctrl Pts',(-25.4366125456109,0.872773089361185,-2.39789925750829));
#7627=CARTESIAN_POINT('Ctrl Pts',(-25.4792624301743,0.895742905086413,-2.38626076145437));
#7628=CARTESIAN_POINT('Ctrl Pts',(-25.5084964623614,0.909714092086876,-2.37894252774089));
#7629=CARTESIAN_POINT('Ctrl Pts',(-25.5535782411859,0.928604376053527,-2.36882359052986));
#7630=CARTESIAN_POINT('Ctrl Pts',(-25.5688259457879,0.934560719395066,-2.36559119630037));
#7631=CARTESIAN_POINT('Ctrl Pts',(-25.5920028890314,0.942960637972606,-2.36098573061775));
#7632=CARTESIAN_POINT('Ctrl Pts',(-25.599788491408,0.945674190484414,-2.35948958119257));
#7633=CARTESIAN_POINT('Ctrl Pts',(-25.6154616875292,0.950919800805258,-2.35658312944662));
#7634=CARTESIAN_POINT('Ctrl Pts',(-25.6233618667185,0.953455374519274,-2.35517084263495));
#7635=CARTESIAN_POINT('Ctrl Pts',(-25.6470880823365,0.960745646595264,-2.35109181935035));
#7636=CARTESIAN_POINT('Ctrl Pts',(-25.6629699013087,0.965196922396597,-2.3485760380501));
#7637=CARTESIAN_POINT('Ctrl Pts',(-25.694878800485,0.973298033223304,-2.34396524772702));
#7638=CARTESIAN_POINT('Ctrl Pts',(-25.7109029793721,0.976947208699529,-2.34187060158446));
#7639=CARTESIAN_POINT('Ctrl Pts',(-25.7591846810364,0.986700310761385,-2.33624184790048));
#7640=CARTESIAN_POINT('Ctrl Pts',(-25.7916509919276,0.991612544814411,-2.33336313702002));
#7641=CARTESIAN_POINT('Ctrl Pts',(-25.8407757493374,0.996579561426926,-2.33044270026262));
#7642=CARTESIAN_POINT('Ctrl Pts',(-25.8572216409297,0.997834347780408,-2.32970209313936));
#7643=CARTESIAN_POINT('Ctrl Pts',(-25.8902579157094,0.99953001979152,-2.32870039378829));
#7644=CARTESIAN_POINT('Ctrl Pts',(-25.9068579008084,0.999970378057446,-2.32843964431104));
#7645=CARTESIAN_POINT('Ctrl Pts',(-25.940167339092,1.00002111583352,-2.3284096204183));
#7646=CARTESIAN_POINT('Ctrl Pts',(-25.9569704089505,0.999625616638201,-2.32864383514006));
#7647=CARTESIAN_POINT('Ctrl Pts',(-25.9903232055858,0.998000175999137,-2.32960420547288));
#7648=CARTESIAN_POINT('Ctrl Pts',(-26.0069063303974,0.996774630505938,-2.33032774135208));
#7649=CARTESIAN_POINT('Ctrl Pts',(-26.0398869194724,0.993513631149881,-2.33224559661821));
#7650=CARTESIAN_POINT('Ctrl Pts',(-26.056285023184,0.991478624792932,-2.33343963815292));
#7651=CARTESIAN_POINT('Ctrl Pts',(-26.0889003945458,0.98661153251092,-2.33628016806539));
#7652=CARTESIAN_POINT('Ctrl Pts',(-26.105117655415,0.98377941166941,-2.33792666122146));
#7653=CARTESIAN_POINT('Ctrl Pts',(-26.1535018144213,0.97409599204652,-2.34351778370754));
#7654=CARTESIAN_POINT('Ctrl Pts',(-26.1854052228443,0.96605741829964,-2.34811578904635));
#7655=CARTESIAN_POINT('Ctrl Pts',(-26.2248338237297,0.954024410911557,-2.35485332977763));
#7656=CARTESIAN_POINT('Ctrl Pts',(-26.2327009185887,0.951515790581765,-2.35625162439446));
#7657=CARTESIAN_POINT('Ctrl Pts',(-26.2483822299402,0.946301415592771,-2.35914306656481));
#7658=CARTESIAN_POINT('Ctrl Pts',(-26.2562112318338,0.943589735649575,-2.36063941300517));
#7659=CARTESIAN_POINT('Ctrl Pts',(-26.2795244997708,0.935189305203656,-2.36524892931282));
#7660=CARTESIAN_POINT('Ctrl Pts',(-26.2948376392117,0.929237415872069,-2.36848154417624));
#7661=CARTESIAN_POINT('Ctrl Pts',(-26.325051496053,0.916635663404135,-2.37523752156304));
#7662=CARTESIAN_POINT('Ctrl Pts',(-26.3399472189906,0.909987758386285,-2.37875982107005));
#7663=CARTESIAN_POINT('Ctrl Pts',(-26.3693282937335,0.896008576234029,-2.38605988196961));
#7664=CARTESIAN_POINT('Ctrl Pts',(-26.3838136313699,0.888677280052345,-2.38983766464246));
#7665=CARTESIAN_POINT('Ctrl Pts',(-26.4123824877164,0.873335934871323,-2.39761699508693));
#7666=CARTESIAN_POINT('Ctrl Pts',(-26.426465999434,0.865325879915263,-2.40161856279579));
#7667=CARTESIAN_POINT('Ctrl Pts',(-26.4542364991726,0.848625856496655,-2.40981481750004));
#7668=CARTESIAN_POINT('Ctrl Pts',(-26.4679235551807,0.839935843967827,-2.4140095472354));
#7669=CARTESIAN_POINT('Ctrl Pts',(-26.4949029725259,0.821869160578012,-2.42256208855009));
#7670=CARTESIAN_POINT('Ctrl Pts',(-26.508198393727,0.812490238648992,-2.42692093963487));
#7671=CARTESIAN_POINT('Ctrl Pts',(-26.5343819518632,0.793041279750162,-2.43576830807168));
#7672=CARTESIAN_POINT('Ctrl Pts',(-26.5471728631521,0.783043916212135,-2.44022370093141));
#7673=CARTESIAN_POINT('Ctrl Pts',(-26.5721858410978,0.7625007828935,-2.44917049567471));
#7674=CARTESIAN_POINT('Ctrl Pts',(-26.5844054044419,0.751956838431777,-2.45366107730755));
#7675=CARTESIAN_POINT('Ctrl Pts',(-26.6082832421287,0.7303277978894,-2.46264578885995));
#7676=CARTESIAN_POINT('Ctrl Pts',(-26.6199414783443,0.719242678452873,-2.46713996742475));
#7677=CARTESIAN_POINT('Ctrl Pts',(-26.654085577301,0.685174209401599,-2.48058330680097));
#7678=CARTESIAN_POINT('Ctrl Pts',(-26.6757450357663,0.661376894583318,-2.48949445887106));
#7679=CARTESIAN_POINT('Ctrl Pts',(-26.7065719269914,0.624020742585242,-2.50260699297805));
#7680=CARTESIAN_POINT('Ctrl Pts',(-26.7165747372154,0.611284460442826,-2.50693773894738));
#7681=CARTESIAN_POINT('Ctrl Pts',(-26.7311521296313,0.591760614150662,-2.51334627463049));
#7682=CARTESIAN_POINT('Ctrl Pts',(-26.7359439235075,0.585177012577667,-2.51546959688903));
#7683=CARTESIAN_POINT('Ctrl Pts',(-26.7453802030872,0.571873056438928,-2.51968170745715));
#7684=CARTESIAN_POINT('Ctrl Pts',(-26.7500338491731,0.565138866716572,-2.52177466043333));
#7685=CARTESIAN_POINT('Ctrl Pts',(-26.7637209428383,0.544802595278455,-2.52797323999353));
#7686=CARTESIAN_POINT('Ctrl Pts',(-26.7724790166661,0.531073974286136,-2.53199736377098));
#7687=CARTESIAN_POINT('Ctrl Pts',(-26.7892933503868,0.503246810054306,-2.53981607542183));
#7688=CARTESIAN_POINT('Ctrl Pts',(-26.7973464004641,0.48915324002206,-2.54360923524379));
#7689=CARTESIAN_POINT('Ctrl Pts',(-26.8204531754343,0.446331963437203,-2.55460789831046));
#7690=CARTESIAN_POINT('Ctrl Pts',(-26.8344570585593,0.417064919965781,-2.56143305219686));
#7691=CARTESIAN_POINT('Ctrl Pts',(-26.8596473785478,0.357056801425753,-2.57389602618922));
#7692=CARTESIAN_POINT('Ctrl Pts',(-26.8708351093533,0.326306410018255,-2.57953500168131));
#7693=CARTESIAN_POINT('Ctrl Pts',(-26.8854188856717,0.279044721282978,-2.58696387685386));
#7694=CARTESIAN_POINT('Ctrl Pts',(-26.889916181885,0.263080008230864,-2.58927006723959));
#7695=CARTESIAN_POINT('Ctrl Pts',(-26.8981455932565,0.230785659439779,-2.59350988787546));
#7696=CARTESIAN_POINT('Ctrl Pts',(-26.9018527777375,0.21455323269401,-2.59543061746581));
#7697=CARTESIAN_POINT('Ctrl Pts',(-26.9084592496751,0.181885630631588,-2.5988657298962));
#7698=CARTESIAN_POINT('Ctrl Pts',(-26.9113559512979,0.165463618176976,-2.60037877253407));
#7699=CARTESIAN_POINT('Ctrl Pts',(-26.9163368119689,0.13239300581574,-2.60298704123574));
#7700=CARTESIAN_POINT('Ctrl Pts',(-26.9184090029522,0.115817353571132,-2.60407599650051));
#7701=CARTESIAN_POINT('Ctrl Pts',(-26.9233578038635,0.0661857319676014,
-2.60668048407778));
#7702=CARTESIAN_POINT('Ctrl Pts',(-26.9249957317331,0.0331163807650845,
-2.60754764115517));
#7703=CARTESIAN_POINT('Ctrl Pts',(-26.9249997882108,-0.0164340525421252,
-2.60754980435114));
#7704=CARTESIAN_POINT('Ctrl Pts',(-26.924592211501,-0.0329434099001476,
-2.60733433932483));
#7705=CARTESIAN_POINT('Ctrl Pts',(-26.922958321114,-0.0659472086648998,
-2.60647188023517));
#7706=CARTESIAN_POINT('Ctrl Pts',(-26.9217320306451,-0.0824416504222753,
-2.60582488664724));
#7707=CARTESIAN_POINT('Ctrl Pts',(-26.9184538736218,-0.115415515405943,
-2.6040995866923));
#7708=CARTESIAN_POINT('Ctrl Pts',(-26.9164009929087,-0.13189841944903,-2.60302074629033));
#7709=CARTESIAN_POINT('Ctrl Pts',(-26.911460595836,-0.164835084256706,-2.60043347726539));
#7710=CARTESIAN_POINT('Ctrl Pts',(-26.9085597921968,-0.181339379062668,
-2.59891817499629));
#7711=CARTESIAN_POINT('Ctrl Pts',(-26.9019928975065,-0.213907595706399,
-2.59550331376099));
#7712=CARTESIAN_POINT('Ctrl Pts',(-26.8983166368945,-0.230050772994295,
-2.59359841481876));
#7713=CARTESIAN_POINT('Ctrl Pts',(-26.8902023083891,-0.262017358841779,
-2.58941709788185));
#7714=CARTESIAN_POINT('Ctrl Pts',(-26.8857631894022,-0.277848484290429,
-2.58714012203648));
#7715=CARTESIAN_POINT('Ctrl Pts',(-26.8713173449163,-0.324894779397646,
-2.5797790328415));
#7716=CARTESIAN_POINT('Ctrl Pts',(-26.8601819442124,-0.355668892391165,
-2.57416342317005));
#7717=CARTESIAN_POINT('Ctrl Pts',(-26.8412486366545,-0.400939993511204,
-2.56479183005489));
#7718=CARTESIAN_POINT('Ctrl Pts',(-26.8345590268073,-0.415893141702949,
-2.56150689497223));
#7719=CARTESIAN_POINT('Ctrl Pts',(-26.823967020712,-0.438089012396736,-2.55635832654132));
#7720=CARTESIAN_POINT('Ctrl Pts',(-26.8203396689083,-0.445455430851165,
-2.55460350724556));
#7721=CARTESIAN_POINT('Ctrl Pts',(-26.8128985600938,-0.460108665512354,
-2.55102277071131));
#7722=CARTESIAN_POINT('Ctrl Pts',(-26.8090795604559,-0.467404628169114,
-2.54919438667112));
#7723=CARTESIAN_POINT('Ctrl Pts',(-26.797394241101,-0.489073962305609,-2.54363152212406));
#7724=CARTESIAN_POINT('Ctrl Pts',(-26.789289060049,-0.503254782620716,-2.53981402566019));
#7725=CARTESIAN_POINT('Ctrl Pts',(-26.7724543674525,-0.531113894213054,
-2.53198595664959));
#7726=CARTESIAN_POINT('Ctrl Pts',(-26.7637261115164,-0.54479019657989,-2.52797594056182));
#7727=CARTESIAN_POINT('Ctrl Pts',(-26.7366204601151,-0.585077837829173,
-2.51569932133657));
#7728=CARTESIAN_POINT('Ctrl Pts',(-26.7173245039422,-0.610949544590535,
-2.50718576295211));
#7729=CARTESIAN_POINT('Ctrl Pts',(-26.6865409768543,-0.648314158915969,
-2.49408419229669));
#7730=CARTESIAN_POINT('Ctrl Pts',(-26.6759726166714,-0.660528085389519,
-2.48966171422195));
#7731=CARTESIAN_POINT('Ctrl Pts',(-26.6542132239272,-0.684474388015635,
-2.48073390605899));
#7732=CARTESIAN_POINT('Ctrl Pts',(-26.6430264626965,-0.696202382055651,
-2.4762302346818));
#7733=CARTESIAN_POINT('Ctrl Pts',(-26.6257563658622,-0.713443816566624,
-2.46942885891314));
#7734=CARTESIAN_POINT('Ctrl Pts',(-26.6199203558455,-0.719129338058233,
-2.46715519418602));
#7735=CARTESIAN_POINT('Ctrl Pts',(-26.6081482145809,-0.730321546007048,
-2.46262131897029));
#7736=CARTESIAN_POINT('Ctrl Pts',(-26.602201292566,-0.735839132509799,-2.46035683871519));
#7737=CARTESIAN_POINT('Ctrl Pts',(-26.5841980514885,-0.752140229430926,
-2.45358395979734));
#7738=CARTESIAN_POINT('Ctrl Pts',(-26.5719627057113,-0.76268889323127,-2.44908952535157));
#7739=CARTESIAN_POINT('Ctrl Pts',(-26.5345850153881,-0.793372503429244,
-2.43572354204093));
#7740=CARTESIAN_POINT('Ctrl Pts',(-26.5087533968938,-0.812566724291243,
-2.42696101356095));
#7741=CARTESIAN_POINT('Ctrl Pts',(-26.4686207796459,-0.839482273044303,
-2.41422655155215));
#7742=CARTESIAN_POINT('Ctrl Pts',(-26.4550114406092,-0.848141391767849,
-2.4100497583254));
#7743=CARTESIAN_POINT('Ctrl Pts',(-26.4273190367366,-0.864830292639691,
-2.40186446327311));
#7744=CARTESIAN_POINT('Ctrl Pts',(-26.4132360104195,-0.872860114977224,
-2.39785591495116));
#7745=CARTESIAN_POINT('Ctrl Pts',(-26.384582055835,-0.888281159414981,-2.39004076104538));
#7746=CARTESIAN_POINT('Ctrl Pts',(-26.3700168965852,-0.895669478070542,
-2.38623564655444));
#7747=CARTESIAN_POINT('Ctrl Pts',(-26.3477718580352,-0.906270310920242,
-2.38070172959633));
#7748=CARTESIAN_POINT('Ctrl Pts',(-26.3402920246762,-0.909722137727464,
-2.3788867625548));
#7749=CARTESIAN_POINT('Ctrl Pts',(-26.3252941333419,-0.9164202866514,-2.37534201103856));
#7750=CARTESIAN_POINT('Ctrl Pts',(-26.3177603512233,-0.919674724840889,
-2.37360807070524));
#7751=CARTESIAN_POINT('Ctrl Pts',(-26.2799597723219,-0.935450414400054,
-2.36515131650746));
#7752=CARTESIAN_POINT('Ctrl Pts',(-26.2492303116149,-0.946538086235367,
-2.35904259359383));
#7753=CARTESIAN_POINT('Ctrl Pts',(-26.1868085832625,-0.965668578368493,
-2.34833591063874));
#7754=CARTESIAN_POINT('Ctrl Pts',(-26.1551124003162,-0.973715224519596,
-2.34373600934578));
#7755=CARTESIAN_POINT('Ctrl Pts',(-26.1068141625445,-0.983466877886542,
-2.33810786542035));
#7756=CARTESIAN_POINT('Ctrl Pts',(-26.0905889199931,-0.986330406808508,
-2.33644376922427));
#7757=CARTESIAN_POINT('Ctrl Pts',(-26.0578798138569,-0.991267004789945,
-2.33356356824837));
#7758=CARTESIAN_POINT('Ctrl Pts',(-26.0413987784432,-0.993339559141272,
-2.33234779729885));
#7759=CARTESIAN_POINT('Ctrl Pts',(-26.0164682576784,-0.995840021233339,
-2.33087747927257));
#7760=CARTESIAN_POINT('Ctrl Pts',(-26.0081136505026,-0.996572064821672,
-2.33044626591382));
#7761=CARTESIAN_POINT('Ctrl Pts',(-25.9914405419907,-0.997822188899729,
-2.3297091449783));
#7762=CARTESIAN_POINT('Ctrl Pts',(-25.983108979154,-0.998341962394754,-2.32940224532968));
#7763=CARTESIAN_POINT('Ctrl Pts',(-25.9581619401288,-0.999585267481811,
-2.32866771122069));
#7764=CARTESIAN_POINT('Ctrl Pts',(-25.9415535530913,-0.999997281825196,
-2.32842370354953));
#7765=CARTESIAN_POINT('Ctrl Pts',(-25.8918801633427,-0.999995995609914,
-2.32842452644233));
#7766=CARTESIAN_POINT('Ctrl Pts',(-25.8588977400795,-0.998354960350017,
-2.32939847806693));
#7767=CARTESIAN_POINT('Ctrl Pts',(-25.809655632564,-0.993459342757443,-2.33227744379061));
#7768=CARTESIAN_POINT('Ctrl Pts',(-25.7932782734797,-0.991421278478376,
-2.33347323218692));
#7769=CARTESIAN_POINT('Ctrl Pts',(-25.7605969584102,-0.986528474355795,
-2.33632851316856));
#7770=CARTESIAN_POINT('Ctrl Pts',(-25.7442875327586,-0.983672349909108,
-2.33798881805762));
#7771=CARTESIAN_POINT('Ctrl Pts',(-25.7198951962202,-0.97877216559872,-2.34081761913493));
#7772=CARTESIAN_POINT('Ctrl Pts',(-25.7117696482312,-0.977034217384623,
-2.34181798163729));
#7773=CARTESIAN_POINT('Ctrl Pts',(-25.6955367491711,-0.973349801421778,
-2.34393091101302));
#7774=CARTESIAN_POINT('Ctrl Pts',(-25.6874344702097,-0.971403984435828,
-2.34504307866984));
#7775=CARTESIAN_POINT('Ctrl Pts',(-25.6632988267017,-0.965288201987582,
-2.34852442457186));
#7776=CARTESIAN_POINT('Ctrl Pts',(-25.6473898327442,-0.960831588438292,
-2.35104334024925));
#7777=CARTESIAN_POINT('Ctrl Pts',(-25.6159256353873,-0.951177087518217,
-2.35644596476354));
#7778=CARTESIAN_POINT('Ctrl Pts',(-25.6003698930602,-0.945979355455216,
-2.35932958924631));
#7779=CARTESIAN_POINT('Ctrl Pts',(-25.5696016033233,-0.934854907919286,
-2.36543090574196));
#7780=CARTESIAN_POINT('Ctrl Pts',(-25.5543890761051,-0.928928152287276,
-2.36864862443056));
#7781=CARTESIAN_POINT('Ctrl Pts',(-25.5092559713361,-0.910063051819414,
-2.37875853937476));
#7782=CARTESIAN_POINT('Ctrl Pts',(-25.4798371327009,-0.896039907812134,
-2.3861084711256));
#7783=CARTESIAN_POINT('Ctrl Pts',(-25.4438916664408,-0.876696452792308,
-2.39591178467008));
#7784=CARTESIAN_POINT('Ctrl Pts',(-25.4367422081294,-0.872734553740174,
-2.39790417870508));
#7785=CARTESIAN_POINT('Ctrl Pts',(-25.4225301197978,-0.864630295332379,
-2.40194577660712));
#7786=CARTESIAN_POINT('Ctrl Pts',(-25.415458892085,-0.860482058534017,-2.40399774819589));
#7787=CARTESIAN_POINT('Ctrl Pts',(-25.3944665440157,-0.84781813222127,-2.41020698379142));
#7788=CARTESIAN_POINT('Ctrl Pts',(-25.3807469194853,-0.839074603637404,
-2.41442221810217));
#7789=CARTESIAN_POINT('Ctrl Pts',(-25.3538269146123,-0.820986612312255,
-2.42297440207295));
#7790=CARTESIAN_POINT('Ctrl Pts',(-25.3406288513095,-0.811643743807895,
-2.42731061510823));
#7791=CARTESIAN_POINT('Ctrl Pts',(-25.3147440120878,-0.792365407430333,
-2.43607078110781));
#7792=CARTESIAN_POINT('Ctrl Pts',(-25.302057253131,-0.782429927595734,-2.44049476170448));
#7793=CARTESIAN_POINT('Ctrl Pts',(-25.2771870451046,-0.761966360498884,
-2.44939937123357));
#7794=CARTESIAN_POINT('Ctrl Pts',(-25.2650036031527,-0.751438272731148,
-2.45388002625663));
#7795=CARTESIAN_POINT('Ctrl Pts',(-25.2411363975391,-0.729784484637608,
-2.4628677672137));
#7796=CARTESIAN_POINT('Ctrl Pts',(-25.2294526316117,-0.718658795136046,
-2.46737487908639));
#7797=CARTESIAN_POINT('Ctrl Pts',(-25.2065854499521,-0.695799709481919,
-2.47638573024674));
#7798=CARTESIAN_POINT('Ctrl Pts',(-25.1954025574532,-0.684066558646475,
-2.48088932142673));
#7799=CARTESIAN_POINT('Ctrl Pts',(-25.1790057014816,-0.665998774177092,
-2.48762031005077));
#7800=CARTESIAN_POINT('Ctrl Pts',(-25.1735972102192,-0.659890699564593,
-2.48986242816921));
#7801=CARTESIAN_POINT('Ctrl Pts',(-25.162950610077,-0.647566600651535,-2.49431653723256));
#7802=CARTESIAN_POINT('Ctrl Pts',(-25.157711714779,-0.641350879252792,-2.49652867473458));
#7803=CARTESIAN_POINT('Ctrl Pts',(-25.1319370754269,-0.609998354557005,
-2.50750690290623));
#7804=CARTESIAN_POINT('Ctrl Pts',(-25.1126444312025,-0.584052119288394,
-2.51602690308558));
#7805=CARTESIAN_POINT('Ctrl Pts',(-25.0766572872409,-0.530427486923969,
-2.53233703039074));
#7806=CARTESIAN_POINT('Ctrl Pts',(-25.059961236299,-0.502749651254318,-2.5401282199127));
#7807=CARTESIAN_POINT('Ctrl Pts',(-25.0368800991623,-0.459893940418667,
-2.5511186769858));
#7808=CARTESIAN_POINT('Ctrl Pts',(-25.0295141239499,-0.445385200926373,
-2.55466616380488));
#7809=CARTESIAN_POINT('Ctrl Pts',(-25.0154489582634,-0.415908528063236,
-2.56150305960081));
#7810=CARTESIAN_POINT('Ctrl Pts',(-25.0087494145486,-0.40093905147491,-2.56479267814123));
#7811=CARTESIAN_POINT('Ctrl Pts',(-24.999213902548,-0.378133256488478,-2.56951273362109));
#7812=CARTESIAN_POINT('Ctrl Pts',(-24.9961168386391,-0.370460488165637,
-2.57105248627293));
#7813=CARTESIAN_POINT('Ctrl Pts',(-24.9901160989215,-0.355044978918729,
-2.57404734396979));
#7814=CARTESIAN_POINT('Ctrl Pts',(-24.9872176813169,-0.34731693891287,-2.57549979202268));
#7815=CARTESIAN_POINT('Ctrl Pts',(-24.978825003649,-0.324068265856262,-2.57972038676599));
#7816=CARTESIAN_POINT('Ctrl Pts',(-24.9736233181388,-0.308461431450075,
-2.5823566152535));
#7817=CARTESIAN_POINT('Ctrl Pts',(-24.9640114746886,-0.277068877280409,
-2.58725544515497));
#7818=CARTESIAN_POINT('Ctrl Pts',(-24.9595988320509,-0.261277274869767,
-2.58951929498313));
#7819=CARTESIAN_POINT('Ctrl Pts',(-24.9515558748387,-0.229503410355288,
-2.59366439634912));
#7820=CARTESIAN_POINT('Ctrl Pts',(-24.9479255650923,-0.213521148150432,
-2.59554565951958));
#7821=CARTESIAN_POINT('Ctrl Pts',(-24.9414489760593,-0.181364697617433,
-2.59891367071842));
#7822=CARTESIAN_POINT('Ctrl Pts',(-24.9386026892397,-0.165190511764201,
-2.60040043074177));
#7823=CARTESIAN_POINT('Ctrl Pts',(-24.9337017706774,-0.132647674346382,
-2.60296683712999));
#7824=CARTESIAN_POINT('Ctrl Pts',(-24.9316471184334,-0.116279028004551,
-2.60404649646001));
#7825=CARTESIAN_POINT('Ctrl Pts',(-24.9283432634801,-0.0833433888462472,
-2.60578520034254));
#7826=CARTESIAN_POINT('Ctrl Pts',(-24.9270943388138,-0.0667755622802253,
-2.60644409327794));
#7827=CARTESIAN_POINT('Ctrl Pts',(-24.9258394406481,-0.0417735825487939,
-2.60710648445229));
#7828=CARTESIAN_POINT('Ctrl Pts',(-24.9255244961035,-0.0334015655269927,
-2.6072728288538));
#7829=CARTESIAN_POINT('Ctrl Pts',(-24.9251056202904,-0.0166741410701568,
-2.60749409590418));
#7830=CARTESIAN_POINT('Ctrl Pts',(-24.9250013822027,-0.00832706674008044,
-2.60754917994845));
#7831=CARTESIAN_POINT('Ctrl Pts',(-24.9250015605239,9.19874578470569E-16,
-2.60754908509523));
#7832=CARTESIAN_POINT('Origin',(-28.425,5.02797759097482E-32,0.));
#7833=CARTESIAN_POINT('',(-28.425,-3.,1.00000000000001));
#7834=CARTESIAN_POINT('Origin',(-28.425,-3.,1.00000000000001));
#7835=CARTESIAN_POINT('',(-21.125,-3.,0.999999999999995));
#7836=CARTESIAN_POINT('Origin',(-21.125,-3.,-1.00000000000001));
#7837=CARTESIAN_POINT('',(-21.125,-3.,-1.00000000000001));
#7838=CARTESIAN_POINT('Origin',(-28.425,-3.,-1.00000000000001));
#7839=CARTESIAN_POINT('',(-28.425,-3.,-1.00000000000001));
#7840=CARTESIAN_POINT('Origin',(-28.425,5.02797759097482E-32,0.));
#7841=CARTESIAN_POINT('',(0.,0.,0.));
#7842=CARTESIAN_POINT('Origin',(-2.51665162595684,-2.97933962373691,-0.00100000000000002));
#7843=CARTESIAN_POINT('',(-1.43590173451363,-2.77445020930684,0.));
#7844=CARTESIAN_POINT('',(-3.22647644353441,-3.81966618427809,0.));
#7845=CARTESIAN_POINT('Origin',(-2.51665162595684,-2.97933962373691,0.));
#7846=CARTESIAN_POINT('',(-1.43590173451363,-2.77445020930684,0.7));
#7847=CARTESIAN_POINT('',(-1.43590173451363,-2.77445020930684,-0.00100000000000002));
#7848=CARTESIAN_POINT('',(-3.22647644353441,-3.81966618427809,0.7));
#7849=CARTESIAN_POINT('Origin',(-2.51665162595684,-2.97933962373691,0.7));
#7850=CARTESIAN_POINT('',(-3.22647644353441,-3.81966618427809,0.7));
#7851=CARTESIAN_POINT('Origin',(1.2766327138965,0.865684251173834,-0.00100000000000002));
#7852=CARTESIAN_POINT('',(0.598421584638982,2.42453949273773,0.));
#7853=CARTESIAN_POINT('',(2.61328937992658,-0.18471993634512,0.));
#7854=CARTESIAN_POINT('Origin',(1.2766327138965,0.865684251173834,0.));
#7855=CARTESIAN_POINT('',(2.61328937992658,-0.18471993634512,0.7));
#7856=CARTESIAN_POINT('',(2.61328937992658,-0.18471993634512,-0.00100000000000002));
#7857=CARTESIAN_POINT('',(0.598421584638982,2.42453949273773,0.7));
#7858=CARTESIAN_POINT('Origin',(1.2766327138965,0.865684251173834,0.7));
#7859=CARTESIAN_POINT('',(0.598421584638982,2.42453949273773,-0.00100000000000002));
#7860=CARTESIAN_POINT('Origin',(0.,0.,0.7));
#7861=CARTESIAN_POINT('',(3.22647644353441,-3.81966618427809,0.7));
#7862=CARTESIAN_POINT('Origin',(0.,0.,0.7));
#7863=CARTESIAN_POINT('',(3.22647644353441,-3.81966618427809,0.));
#7864=CARTESIAN_POINT('',(3.22647644353441,-3.81966618427809,0.7));
#7865=CARTESIAN_POINT('Origin',(0.,0.,0.));
#7866=CARTESIAN_POINT('Origin',(0.,0.,0.7));
#7867=CARTESIAN_POINT('',(1.43590173451363,-2.77445020930684,0.7));
#7868=CARTESIAN_POINT('Origin',(7.33090114238568,-3.89202883347084,0.7));
#7869=CARTESIAN_POINT('Origin',(2.51665162595684,-2.97933962373691,0.7));
#7870=CARTESIAN_POINT('',(-2.61328937992658,-0.18471993634512,0.7));
#7871=CARTESIAN_POINT('Origin',(-7.33090114238567,-3.89202883347085,0.7));
#7872=CARTESIAN_POINT('',(-0.598421584638982,2.42453949273774,0.7));
#7873=CARTESIAN_POINT('Origin',(-1.2766327138965,0.865684251173833,0.7));
#7874=CARTESIAN_POINT('Origin',(0.,3.8,0.7));
#7875=CARTESIAN_POINT('Origin',(0.,0.,0.));
#7876=CARTESIAN_POINT('',(1.43590173451363,-2.77445020930684,0.));
#7877=CARTESIAN_POINT('Origin',(2.51665162595684,-2.97933962373691,0.));
#7878=CARTESIAN_POINT('Origin',(7.33090114238568,-3.89202883347084,0.));
#7879=CARTESIAN_POINT('',(-0.598421584638982,2.42453949273774,0.));
#7880=CARTESIAN_POINT('Origin',(0.,3.8,0.));
#7881=CARTESIAN_POINT('',(-2.61328937992658,-0.18471993634512,0.));
#7882=CARTESIAN_POINT('Origin',(-1.2766327138965,0.865684251173833,0.));
#7883=CARTESIAN_POINT('Origin',(-7.33090114238567,-3.89202883347085,0.));
#7884=CARTESIAN_POINT('Origin',(-1.2766327138965,0.865684251173833,-0.00100000000000002));
#7885=CARTESIAN_POINT('',(-0.598421584638982,2.42453949273774,-0.00100000000000002));
#7886=CARTESIAN_POINT('',(-2.61328937992658,-0.18471993634512,-0.00100000000000002));
#7887=CARTESIAN_POINT('Origin',(0.,3.8,-0.00100000000000002));
#7888=CARTESIAN_POINT('Origin',(7.33090114238568,-3.89202883347084,-0.00100000000000002));
#7889=CARTESIAN_POINT('',(1.43590173451363,-2.77445020930684,-0.00100000000000002));
#7890=CARTESIAN_POINT('Origin',(-7.33090114238567,-3.89202883347085,-0.00100000000000002));
#7891=CARTESIAN_POINT('Origin',(2.51665162595684,-2.97933962373691,0.7));
#7892=CARTESIAN_POINT('',(0.,0.,0.));
#7893=CARTESIAN_POINT('Origin',(0.,0.2,0.));
#7894=CARTESIAN_POINT('',(-1.40834381901946E-16,0.2,1.15));
#7895=CARTESIAN_POINT('Origin',(0.,0.2,0.));
#7896=CARTESIAN_POINT('',(-1.65327317884893E-16,-1.04083408558608E-16,1.35));
#7897=CARTESIAN_POINT('',(-1.40834381901946E-16,0.2,1.15));
#7898=CARTESIAN_POINT('Origin',(0.,0.,0.));
#7899=CARTESIAN_POINT('Origin',(0.,4.85,0.));
#7900=CARTESIAN_POINT('',(-1.40834381901946E-16,4.85,1.15));
#7901=CARTESIAN_POINT('Origin',(0.,4.85,0.));
#7902=CARTESIAN_POINT('',(-1.40834381901946E-16,4.85,1.15));
#7903=CARTESIAN_POINT('Origin',(0.,0.0499999999999997,0.));
#7904=CARTESIAN_POINT('',(0.858631047345558,0.,2.56422556038549));
#7905=CARTESIAN_POINT('',(-0.858631047345558,0.,2.56422556038549));
#7906=CARTESIAN_POINT('Origin',(0.,0.,0.));
#7907=CARTESIAN_POINT('',(0.865846434298039,0.00546218487394905,2.58577367433831));
#7908=CARTESIAN_POINT('Origin',(0.858631047345555,0.0499999999999995,2.56422556038549));
#7909=CARTESIAN_POINT('',(-0.865846434298039,0.00546218487394904,2.58577367433831));
#7910=CARTESIAN_POINT('Origin',(0.,0.00546218487394896,0.));
#7911=CARTESIAN_POINT('Origin',(-0.858631047345558,0.05,2.56422556038549));
#7912=CARTESIAN_POINT('Origin',(2.16840434497101E-16,2.45,-3.05995642670502));
#7913=CARTESIAN_POINT('',(-0.025,2.20285867594495,-3.10325769689424));
#7914=CARTESIAN_POINT('',(0.0250000000000005,2.20285867594495,-3.10325769689424));
#7915=CARTESIAN_POINT('Origin',(4.60785923306339E-16,2.20285867594495,-3.05995642670502));
#7916=CARTESIAN_POINT('',(0.0250000000000005,0.247141324055048,-3.10325769689424));
#7917=CARTESIAN_POINT('',(0.0250000000000005,2.45,-3.10325769689424));
#7918=CARTESIAN_POINT('',(-0.025,0.247141324055048,-3.10325769689424));
#7919=CARTESIAN_POINT('Origin',(-1.01643953670516E-17,0.247141324055048,
-3.05995642670502));
#7920=CARTESIAN_POINT('',(-0.0250000000000001,2.45,-3.10325769689424));
#7921=CARTESIAN_POINT('Origin',(0.,2.4,0.));
#7922=CARTESIAN_POINT('',(0.865846434298034,2.44453781512605,2.58577367433831));
#7923=CARTESIAN_POINT('',(-0.865846434298034,2.44453781512605,2.58577367433831));
#7924=CARTESIAN_POINT('Origin',(0.,2.44453781512605,0.));
#7925=CARTESIAN_POINT('',(0.858631047345553,2.45,2.56422556038549));
#7926=CARTESIAN_POINT('Origin',(0.858631047345553,2.4,2.56422556038549));
#7927=CARTESIAN_POINT('',(-0.858631047345553,2.45,2.56422556038549));
#7928=CARTESIAN_POINT('Origin',(0.,2.45,0.));
#7929=CARTESIAN_POINT('Origin',(-0.85863104734555,2.4,2.56422556038549));
#7930=CARTESIAN_POINT('Origin',(0.,3.025,0.));
#7931=CARTESIAN_POINT('',(3.09223316784707E-16,3.025,2.525));
#7932=CARTESIAN_POINT('Origin',(0.,3.025,0.));
#7933=CARTESIAN_POINT('',(1.8934467256106E-32,5.55,1.54611658392353E-16));
#7934=CARTESIAN_POINT('Origin',(0.,3.025,0.));
#7935=CARTESIAN_POINT('Origin',(0.,5.55,0.));
#7936=CARTESIAN_POINT('',(-3.09223316784707E-16,2.45,2.525));
#7937=CARTESIAN_POINT('Origin',(0.,2.45,0.));
#7938=CARTESIAN_POINT('',(-3.09223316784707E-16,5.55,2.525));
#7939=CARTESIAN_POINT('Origin',(0.,5.35,0.));
#7940=CARTESIAN_POINT('',(-2.67226890756303,0.00546218487394984,0.543041829290872));
#7941=CARTESIAN_POINT('',(-1.80642247326498,0.00546218487394976,2.04273184504743));
#7942=CARTESIAN_POINT('Origin',(0.,0.00546218487394983,0.));
#7943=CARTESIAN_POINT('',(-2.67226890756303,0.204260158710973,1.54283517312858));
#7944=CARTESIAN_POINT('Origin',(-1.33613445378151,5.35,2.31425275969287));
#7945=CARTESIAN_POINT('Origin',(-2.67226890756303,5.35,0.));
#7946=CARTESIAN_POINT('Origin',(0.,5.35,0.));
#7947=CARTESIAN_POINT('',(2.67226890756303,0.00546218487394984,-0.543041829290872));
#7948=CARTESIAN_POINT('',(1.80642247326498,0.00546218487394912,-2.04273184504743));
#7949=CARTESIAN_POINT('Origin',(0.,0.00546218487394983,0.));
#7950=CARTESIAN_POINT('',(2.67226890756303,0.204260158710974,-1.54283517312858));
#7951=CARTESIAN_POINT('Origin',(1.33613445378151,5.35,-2.31425275969287));
#7952=CARTESIAN_POINT('Origin',(2.67226890756303,5.35,0.));
#7953=CARTESIAN_POINT('Origin',(0.,-2.9,0.));
#7954=CARTESIAN_POINT('',(-1.80642247326499,2.44453781512605,2.04273184504743));
#7955=CARTESIAN_POINT('',(-2.67226890756303,2.44453781512605,0.543041829290881));
#7956=CARTESIAN_POINT('Origin',(0.,2.44453781512605,0.));
#7957=CARTESIAN_POINT('',(-2.67226890756303,2.24573984128903,1.54283517312858));
#7958=CARTESIAN_POINT('Origin',(-2.67226890756303,-2.9,0.));
#7959=CARTESIAN_POINT('Origin',(-1.33613445378151,-2.9,2.31425275969287));
#7960=CARTESIAN_POINT('Origin',(0.,-2.9,0.));
#7961=CARTESIAN_POINT('',(1.80642247326499,2.44453781512605,-2.04273184504743));
#7962=CARTESIAN_POINT('',(2.67226890756303,2.44453781512605,-0.543041829290881));
#7963=CARTESIAN_POINT('Origin',(0.,2.44453781512605,0.));
#7964=CARTESIAN_POINT('',(2.67226890756303,2.24573984128903,-1.54283517312858));
#7965=CARTESIAN_POINT('Origin',(2.67226890756303,-2.9,0.));
#7966=CARTESIAN_POINT('Origin',(1.33613445378151,-2.9,-2.31425275969287));
#7967=CARTESIAN_POINT('Origin',(-2.7,2.45,0.));
#7968=CARTESIAN_POINT('',(-2.7,2.20285867594495,-1.52997821335251));
#7969=CARTESIAN_POINT('',(-2.7,0.247141324055048,-1.52997821335251));
#7970=CARTESIAN_POINT('',(-2.7,2.45,-1.52997821335251));
#7971=CARTESIAN_POINT('',(-2.7,0.05,-0.538516480713451));
#7972=CARTESIAN_POINT('Origin',(-2.7,5.35,0.));
#7973=CARTESIAN_POINT('',(-2.7,0.05,0.538516480713451));
#7974=CARTESIAN_POINT('',(-2.7,0.05,0.295803989154973));
#7975=CARTESIAN_POINT('',(-2.7,0.247141324055048,1.52997821335251));
#7976=CARTESIAN_POINT('Origin',(-2.7,5.35,0.));
#7977=CARTESIAN_POINT('',(-2.7,2.20285867594495,1.52997821335251));
#7978=CARTESIAN_POINT('',(-2.7,2.45,1.52997821335251));
#7979=CARTESIAN_POINT('',(-2.7,2.4,0.538516480713459));
#7980=CARTESIAN_POINT('Origin',(-2.7,-2.9,0.));
#7981=CARTESIAN_POINT('',(-2.7,2.4,-0.538516480713458));
#7982=CARTESIAN_POINT('',(-2.7,2.4,0.));
#7983=CARTESIAN_POINT('Origin',(-2.7,-2.9,0.));
#7984=CARTESIAN_POINT('Origin',(-1.35,2.45,2.33826859021798));
#7985=CARTESIAN_POINT('',(-2.675,0.247141324055048,1.57327948354173));
#7986=CARTESIAN_POINT('',(-1.81636895265444,0.0499999999999984,2.06901034986126));
#7987=CARTESIAN_POINT('Origin',(-1.35,5.35,2.33826859021798));
#7988=CARTESIAN_POINT('',(-0.883631047345559,0.0499999999999988,2.60752683057471));
#7989=CARTESIAN_POINT('',(-1.09382623085102,0.05,2.48617058479547));
#7990=CARTESIAN_POINT('',(-0.025,0.247141324055048,3.10325769689424));
#7991=CARTESIAN_POINT('Origin',(-1.35,5.35,2.33826859021798));
#7992=CARTESIAN_POINT('',(-0.025,2.20285867594495,3.10325769689424));
#7993=CARTESIAN_POINT('',(-0.0250000000000001,2.45,3.10325769689424));
#7994=CARTESIAN_POINT('',(-0.883631047345551,2.4,2.60752683057471));
#7995=CARTESIAN_POINT('Origin',(-1.35,-2.9,2.33826859021798));
#7996=CARTESIAN_POINT('',(-1.81636895265445,2.4,2.06901034986126));
#7997=CARTESIAN_POINT('',(-1.35,2.4,2.33826859021798));
#7998=CARTESIAN_POINT('',(-2.675,2.20285867594495,1.57327948354173));
#7999=CARTESIAN_POINT('Origin',(-1.35,-2.9,2.33826859021798));
#8000=CARTESIAN_POINT('',(-2.675,2.45,1.57327948354173));
#8001=CARTESIAN_POINT('Origin',(1.35,2.45,2.33826859021798));
#8002=CARTESIAN_POINT('',(0.0250000000000002,0.247141324055048,3.10325769689424));
#8003=CARTESIAN_POINT('',(0.883631047345559,0.0499999999999988,2.60752683057471));
#8004=CARTESIAN_POINT('Origin',(1.35,5.35,2.33826859021798));
#8005=CARTESIAN_POINT('',(1.81636895265444,0.0499999999999985,2.06901034986126));
#8006=CARTESIAN_POINT('',(1.60617376914898,0.05,2.1903665956405));
#8007=CARTESIAN_POINT('',(2.675,0.247141324055048,1.57327948354173));
#8008=CARTESIAN_POINT('Origin',(1.35,5.35,2.33826859021798));
#8009=CARTESIAN_POINT('',(2.675,2.20285867594495,1.57327948354173));
#8010=CARTESIAN_POINT('',(2.675,2.45,1.57327948354173));
#8011=CARTESIAN_POINT('',(1.81636895265445,2.4,2.06901034986126));
#8012=CARTESIAN_POINT('Origin',(1.35,-2.9,2.33826859021798));
#8013=CARTESIAN_POINT('',(0.883631047345552,2.4,2.60752683057471));
#8014=CARTESIAN_POINT('',(1.35,2.4,2.33826859021798));
#8015=CARTESIAN_POINT('',(0.0250000000000002,2.20285867594495,3.10325769689424));
#8016=CARTESIAN_POINT('Origin',(1.35,-2.9,2.33826859021798));
#8017=CARTESIAN_POINT('',(0.0250000000000003,2.45,3.10325769689424));
#8018=CARTESIAN_POINT('Origin',(2.7,2.45,0.));
#8019=CARTESIAN_POINT('',(2.7,2.20285867594495,-1.52997821335251));
#8020=CARTESIAN_POINT('',(2.7,2.4,-0.538516480713459));
#8021=CARTESIAN_POINT('Origin',(2.7,-2.9,0.));
#8022=CARTESIAN_POINT('',(2.7,2.4,0.538516480713459));
#8023=CARTESIAN_POINT('',(2.7,2.4,0.));
#8024=CARTESIAN_POINT('',(2.7,2.20285867594495,1.52997821335251));
#8025=CARTESIAN_POINT('Origin',(2.7,-2.9,0.));
#8026=CARTESIAN_POINT('',(2.7,0.247141324055047,1.52997821335251));
#8027=CARTESIAN_POINT('',(2.7,2.45,1.52997821335251));
#8028=CARTESIAN_POINT('',(2.7,0.05,0.538516480713451));
#8029=CARTESIAN_POINT('Origin',(2.7,5.35,0.));
#8030=CARTESIAN_POINT('',(2.7,0.05,-0.538516480713451));
#8031=CARTESIAN_POINT('',(2.7,0.05,-0.295803989154973));
#8032=CARTESIAN_POINT('',(2.7,0.247141324055048,-1.52997821335251));
#8033=CARTESIAN_POINT('Origin',(2.7,5.35,0.));
#8034=CARTESIAN_POINT('',(2.7,2.45,-1.52997821335251));
#8035=CARTESIAN_POINT('Origin',(1.35,2.45,-2.33826859021798));
#8036=CARTESIAN_POINT('',(0.883631047345552,2.4,-2.60752683057471));
#8037=CARTESIAN_POINT('Origin',(1.35,-2.9,-2.33826859021798));
#8038=CARTESIAN_POINT('',(1.81636895265445,2.4,-2.06901034986126));
#8039=CARTESIAN_POINT('',(1.35,2.4,-2.33826859021798));
#8040=CARTESIAN_POINT('',(2.675,2.20285867594495,-1.57327948354173));
#8041=CARTESIAN_POINT('Origin',(1.35,-2.9,-2.33826859021798));
#8042=CARTESIAN_POINT('',(2.675,0.247141324055048,-1.57327948354173));
#8043=CARTESIAN_POINT('',(2.675,2.45,-1.57327948354173));
#8044=CARTESIAN_POINT('',(1.81636895265444,0.0499999999999992,-2.06901034986126));
#8045=CARTESIAN_POINT('Origin',(1.35,5.35,-2.33826859021798));
#8046=CARTESIAN_POINT('',(0.883631047345561,0.0499999999999995,-2.60752683057471));
#8047=CARTESIAN_POINT('',(1.09382623085102,0.05,-2.48617058479547));
#8048=CARTESIAN_POINT('Origin',(1.35,5.35,-2.33826859021798));
#8049=CARTESIAN_POINT('Origin',(-1.35,2.45,-2.33826859021798));
#8050=CARTESIAN_POINT('',(-2.675,2.20285867594495,-1.57327948354173));
#8051=CARTESIAN_POINT('',(-1.81636895265445,2.4,-2.06901034986126));
#8052=CARTESIAN_POINT('Origin',(-1.35,-2.9,-2.33826859021798));
#8053=CARTESIAN_POINT('',(-0.883631047345552,2.4,-2.60752683057471));
#8054=CARTESIAN_POINT('',(-1.35,2.4,-2.33826859021798));
#8055=CARTESIAN_POINT('Origin',(-1.35,-2.9,-2.33826859021798));
#8056=CARTESIAN_POINT('',(-0.883631047345559,0.0499999999999987,-2.60752683057471));
#8057=CARTESIAN_POINT('Origin',(-1.35,5.35,-2.33826859021798));
#8058=CARTESIAN_POINT('',(-1.81636895265444,0.0499999999999985,-2.06901034986126));
#8059=CARTESIAN_POINT('',(-1.60617376914898,0.05,-2.1903665956405));
#8060=CARTESIAN_POINT('',(-2.675,0.247141324055048,-1.57327948354173));
#8061=CARTESIAN_POINT('Origin',(-1.35,5.35,-2.33826859021798));
#8062=CARTESIAN_POINT('',(-2.675,2.45,-1.57327948354173));
#8063=CARTESIAN_POINT('Origin',(0.,2.45,0.));
#8064=CARTESIAN_POINT('',(-2.65000000000324,2.45,-0.595818764376248));
#8065=CARTESIAN_POINT('',(-1.84099418601376,2.45,-1.99705793783344));
#8066=CARTESIAN_POINT('Origin',(0.,2.45,0.));
#8067=CARTESIAN_POINT('',(-2.65,2.45,0.538516480713456));
#8068=CARTESIAN_POINT('',(-2.65,2.45,0.));
#8069=CARTESIAN_POINT('',(-1.79136895265445,2.45,2.02570907967203));
#8070=CARTESIAN_POINT('Origin',(0.,2.45,0.));
#8071=CARTESIAN_POINT('',(-1.325,2.45,2.29496732002876));
#8072=CARTESIAN_POINT('',(1.79136895265445,2.45,2.02570907967203));
#8073=CARTESIAN_POINT('',(1.325,2.45,2.29496732002876));
#8074=CARTESIAN_POINT('',(2.65,2.45,0.538516480713456));
#8075=CARTESIAN_POINT('Origin',(0.,2.45,0.));
#8076=CARTESIAN_POINT('',(2.65,2.45,-0.538516480713456));
#8077=CARTESIAN_POINT('',(2.65,2.45,0.));
#8078=CARTESIAN_POINT('',(1.79136895265445,2.45,-2.02570907967203));
#8079=CARTESIAN_POINT('Origin',(0.,2.45,0.));
#8080=CARTESIAN_POINT('',(0.858631047345553,2.45,-2.56422556038549));
#8081=CARTESIAN_POINT('',(1.325,2.45,-2.29496732002876));
#8082=CARTESIAN_POINT('',(-0.858631047345553,2.45,-2.56422556038549));
#8083=CARTESIAN_POINT('Origin',(0.,2.45,0.));
#8084=CARTESIAN_POINT('',(-1.325,2.45,-2.29496732002876));
#8085=CARTESIAN_POINT('Origin',(0.,0.,0.));
#8086=CARTESIAN_POINT('',(2.65,0.,-0.538516480713445));
#8087=CARTESIAN_POINT('',(2.65,0.,0.538516480713445));
#8088=CARTESIAN_POINT('',(2.65,0.,0.295803989154973));
#8089=CARTESIAN_POINT('',(1.79136895265444,0.,2.02570907967204));
#8090=CARTESIAN_POINT('Origin',(0.,0.,0.));
#8091=CARTESIAN_POINT('',(1.06882623085102,0.,2.44286931460625));
#8092=CARTESIAN_POINT('',(-1.79136895265444,0.,2.02570907967204));
#8093=CARTESIAN_POINT('',(-1.58117376914898,0.,2.14706532545128));
#8094=CARTESIAN_POINT('',(-2.65,0.,0.538516480713445));
#8095=CARTESIAN_POINT('Origin',(0.,0.,0.));
#8096=CARTESIAN_POINT('',(-2.65,0.,-0.538516480713445));
#8097=CARTESIAN_POINT('',(-2.65,0.,-0.295803989154973));
#8098=CARTESIAN_POINT('',(-1.79136895265444,0.,-2.02570907967204));
#8099=CARTESIAN_POINT('Origin',(0.,0.,0.));
#8100=CARTESIAN_POINT('',(-0.858631047345558,0.,-2.56422556038549));
#8101=CARTESIAN_POINT('',(-1.06882623085102,0.,-2.44286931460625));
#8102=CARTESIAN_POINT('',(0.858631047345562,0.,-2.56422556038549));
#8103=CARTESIAN_POINT('Origin',(0.,0.,0.));
#8104=CARTESIAN_POINT('',(1.79136895265444,0.,-2.02570907967204));
#8105=CARTESIAN_POINT('',(1.58117376914898,0.,-2.14706532545128));
#8106=CARTESIAN_POINT('Origin',(0.,0.,0.));
#8107=CARTESIAN_POINT('Origin',(0.,-2.9,0.));
#8108=CARTESIAN_POINT('',(1.59968345746445E-16,2.24573984128903,3.08567034625716));
#8109=CARTESIAN_POINT('Origin',(-1.33613445378151,-2.9,2.31425275969287));
#8110=CARTESIAN_POINT('Origin',(1.33613445378151,-2.9,2.31425275969287));
#8111=CARTESIAN_POINT('Origin',(0.,-2.9,0.));
#8112=CARTESIAN_POINT('',(1.80642247326499,2.44453781512605,2.04273184504743));
#8113=CARTESIAN_POINT('',(2.67226890756303,2.24573984128903,1.54283517312858));
#8114=CARTESIAN_POINT('Origin',(1.33613445378151,-2.9,2.31425275969287));
#8115=CARTESIAN_POINT('',(2.67226890756303,2.44453781512605,0.543041829290881));
#8116=CARTESIAN_POINT('Origin',(2.67226890756303,-2.9,0.));
#8117=CARTESIAN_POINT('Origin',(0.,2.44453781512605,0.));
#8118=CARTESIAN_POINT('Origin',(0.,-2.9,0.));
#8119=CARTESIAN_POINT('',(0.865846434298035,2.44453781512605,-2.58577367433831));
#8120=CARTESIAN_POINT('',(6.63014680110683E-16,2.24573984128903,-3.08567034625716));
#8121=CARTESIAN_POINT('Origin',(1.33613445378151,-2.9,-2.31425275969287));
#8122=CARTESIAN_POINT('',(-0.865846434298034,2.44453781512605,-2.58577367433831));
#8123=CARTESIAN_POINT('Origin',(-1.33613445378151,-2.9,-2.31425275969287));
#8124=CARTESIAN_POINT('Origin',(0.,2.44453781512605,0.));
#8125=CARTESIAN_POINT('Origin',(0.,-2.9,0.));
#8126=CARTESIAN_POINT('',(-2.67226890756303,2.24573984128903,-1.54283517312858));
#8127=CARTESIAN_POINT('',(-2.67226890756303,2.4447671280735,-0.540780207049814));
#8128=CARTESIAN_POINT('Origin',(-2.67226890756303,-2.9,0.));
#8129=CARTESIAN_POINT('Ctrl Pts',(-2.67226890756303,2.4447671280735,-0.540780207049819));
#8130=CARTESIAN_POINT('Ctrl Pts',(-2.67188165522803,2.44495976241979,-0.540789927546888));
#8131=CARTESIAN_POINT('Ctrl Pts',(-2.67148794036228,2.44514904528708,-0.54086418367862));
#8132=CARTESIAN_POINT('Ctrl Pts',(-2.67038852238207,2.44566128822559,-0.541231202677014));
#8133=CARTESIAN_POINT('Ctrl Pts',(-2.66970822201384,2.44595619716623,-0.541674224166172));
#8134=CARTESIAN_POINT('Ctrl Pts',(-2.66561324339082,2.44765239284951,-0.545108397107626));
#8135=CARTESIAN_POINT('Ctrl Pts',(-2.66401855855887,2.44802977908222,-0.549184489970353));
#8136=CARTESIAN_POINT('Ctrl Pts',(-2.66047421567082,2.44892435679286,-0.557589611972086));
#8137=CARTESIAN_POINT('Ctrl Pts',(-2.65893507904906,2.44921707503779,-0.562108065848044));
#8138=CARTESIAN_POINT('Ctrl Pts',(-2.65458003737285,2.44987629703967,-0.576304280926598));
#8139=CARTESIAN_POINT('Ctrl Pts',(-2.65211510888084,2.45,-0.586411476689759));
#8140=CARTESIAN_POINT('Ctrl Pts',(-2.65,2.45,-0.595818764390658));
#8141=CARTESIAN_POINT('',(-1.80446385095045,2.4447671280735,-2.04386265616796));
#8142=CARTESIAN_POINT('Ctrl Pts',(-1.84099418601376,2.45,-1.99705793783343));
#8143=CARTESIAN_POINT('Ctrl Pts',(-1.8339047903245,2.45,-2.00359331970646));
#8144=CARTESIAN_POINT('Ctrl Pts',(-1.82638416627859,2.44987629703967,-2.01078160828064));
#8145=CARTESIAN_POINT('Ctrl Pts',(-1.81626740422107,2.44921707503779,-2.02165129254605));
#8146=CARTESIAN_POINT('Ctrl Pts',(-1.81312387668954,2.44892435679286,-2.02524345089836));
#8147=CARTESIAN_POINT('Ctrl Pts',(-1.80761699895816,2.44802977908222,-2.03251550288001));
#8148=CARTESIAN_POINT('Ctrl Pts',(-1.80488434140683,2.44765239284951,-2.03593458688687));
#8149=CARTESIAN_POINT('Ctrl Pts',(-1.80395774971005,2.44595619716623,-2.04119802887309));
#8150=CARTESIAN_POINT('Ctrl Pts',(-1.80391423203013,2.44566128822559,-2.04200869701876));
#8151=CARTESIAN_POINT('Ctrl Pts',(-1.80414609324395,2.44514904528708,-2.04314433041819));
#8152=CARTESIAN_POINT('Ctrl Pts',(-1.80427864298037,2.44495976241979,-2.04352242555965));
#8153=CARTESIAN_POINT('Ctrl Pts',(-1.80446385095046,2.4447671280735,-2.04386265616796));
#8154=CARTESIAN_POINT('Origin',(-1.33613445378151,-2.9,-2.31425275969287));
#8155=CARTESIAN_POINT('Origin',(0.,5.35,0.));
#8156=CARTESIAN_POINT('',(2.41574498103394E-16,0.204260158710972,3.08567034625716));
#8157=CARTESIAN_POINT('Origin',(1.33613445378151,5.35,2.31425275969287));
#8158=CARTESIAN_POINT('Origin',(-1.33613445378151,5.35,2.31425275969287));
#8159=CARTESIAN_POINT('Origin',(0.,5.35,0.));
#8160=CARTESIAN_POINT('',(1.80642247326498,0.00546218487394966,2.04273184504743));
#8161=CARTESIAN_POINT('',(2.67226890756303,0.00546218487394974,0.543041829290871));
#8162=CARTESIAN_POINT('Origin',(0.,0.00546218487394983,0.));
#8163=CARTESIAN_POINT('',(2.67226890756303,0.204260158710973,1.54283517312858));
#8164=CARTESIAN_POINT('Origin',(2.67226890756303,5.35,0.));
#8165=CARTESIAN_POINT('Origin',(1.33613445378151,5.35,2.31425275969287));
#8166=CARTESIAN_POINT('Origin',(0.,5.35,0.));
#8167=CARTESIAN_POINT('',(0.865846434298044,0.00546218487394985,-2.58577367433831));
#8168=CARTESIAN_POINT('',(-0.865846434298039,0.00546218487394872,-2.58577367433831));
#8169=CARTESIAN_POINT('Origin',(0.,0.00546218487394896,0.));
#8170=CARTESIAN_POINT('',(8.28890235087106E-16,0.204260158710973,-3.08567034625716));
#8171=CARTESIAN_POINT('Origin',(-1.33613445378151,5.35,-2.31425275969287));
#8172=CARTESIAN_POINT('Origin',(1.33613445378151,5.35,-2.31425275969287));
#8173=CARTESIAN_POINT('Origin',(0.,5.35,0.));
#8174=CARTESIAN_POINT('',(-1.80642247326498,0.00546218487394966,-2.04273184504743));
#8175=CARTESIAN_POINT('',(-2.67226890756303,0.00546218487394972,-0.543041829290871));
#8176=CARTESIAN_POINT('Origin',(0.,0.00546218487394983,0.));
#8177=CARTESIAN_POINT('',(-2.67226890756303,0.204260158710973,-1.54283517312858));
#8178=CARTESIAN_POINT('Origin',(-2.67226890756303,5.35,0.));
#8179=CARTESIAN_POINT('Origin',(-1.33613445378151,5.35,-2.31425275969287));
#8180=CARTESIAN_POINT('Origin',(2.65,2.4,0.538516480713455));
#8181=CARTESIAN_POINT('Origin',(2.65,2.4,0.538516480713457));
#8182=CARTESIAN_POINT('Origin',(2.65,2.4,0.538516480713459));
#8183=CARTESIAN_POINT('Origin',(2.65,2.4,0.538516480713456));
#8184=CARTESIAN_POINT('Origin',(2.65,2.4,0.));
#8185=CARTESIAN_POINT('Origin',(2.65,2.4,-0.538516480713456));
#8186=CARTESIAN_POINT('Origin',(0.,2.4,0.));
#8187=CARTESIAN_POINT('Origin',(1.79136895265445,2.4,2.02570907967203));
#8188=CARTESIAN_POINT('Origin',(1.325,-2.9,2.29496732002876));
#8189=CARTESIAN_POINT('Origin',(2.65,2.20285867594495,1.52997821335251));
#8190=CARTESIAN_POINT('Origin',(1.79136895265445,2.4,2.02570907967203));
#8191=CARTESIAN_POINT('Origin',(2.65,-2.9,0.));
#8192=CARTESIAN_POINT('Origin',(2.65,2.20285867594495,1.52997821335251));
#8193=CARTESIAN_POINT('Origin',(2.65,-2.9,0.));
#8194=CARTESIAN_POINT('Origin',(2.65,2.4,-0.538516480713459));
#8195=CARTESIAN_POINT('Origin',(2.65,2.20285867594495,-1.52997821335251));
#8196=CARTESIAN_POINT('Origin',(2.65,2.4,-0.538516480713455));
#8197=CARTESIAN_POINT('Origin',(2.65,2.4,-0.538516480713457));
#8198=CARTESIAN_POINT('Origin',(1.79136895265445,2.4,2.02570907967203));
#8199=CARTESIAN_POINT('Origin',(1.79136895265445,2.4,2.02570907967203));
#8200=CARTESIAN_POINT('Origin',(2.65,2.20285867594495,1.52997821335251));
#8201=CARTESIAN_POINT('Origin',(2.65,2.20285867594495,1.52997821335251));
#8202=CARTESIAN_POINT('Origin',(2.65,2.20285867594495,-1.52997821335251));
#8203=CARTESIAN_POINT('Origin',(2.65,2.20285867594495,-1.52997821335251));
#8204=CARTESIAN_POINT('Origin',(2.65,2.20285867594495,-1.52997821335251));
#8205=CARTESIAN_POINT('Origin',(1.325,-2.9,-2.29496732002876));
#8206=CARTESIAN_POINT('Origin',(1.79136895265445,2.4,-2.02570907967203));
#8207=CARTESIAN_POINT('Origin',(0.,2.4,0.));
#8208=CARTESIAN_POINT('Origin',(1.79136895265445,2.4,-2.02570907967203));
#8209=CARTESIAN_POINT('Origin',(1.325,2.4,2.29496732002876));
#8210=CARTESIAN_POINT('Origin',(0.858631047345551,2.4,2.56422556038549));
#8211=CARTESIAN_POINT('Origin',(2.65,2.45,1.52997821335251));
#8212=CARTESIAN_POINT('Origin',(2.65,0.247141324055047,1.52997821335251));
#8213=CARTESIAN_POINT('Origin',(2.65,5.35,0.));
#8214=CARTESIAN_POINT('Origin',(2.65,0.05,0.538516480713451));
#8215=CARTESIAN_POINT('Origin',(2.65,0.247141324055048,1.52997821335251));
#8216=CARTESIAN_POINT('Origin',(2.65,0.05,0.));
#8217=CARTESIAN_POINT('Origin',(2.65,0.05,-0.538516480713451));
#8218=CARTESIAN_POINT('Origin',(2.65,0.05,0.538516480713445));
#8219=CARTESIAN_POINT('Origin',(2.65,5.35,0.));
#8220=CARTESIAN_POINT('Origin',(2.65,0.247141324055048,-1.52997821335251));
#8221=CARTESIAN_POINT('Origin',(2.65,0.0500000000000003,-0.538516480713448));
#8222=CARTESIAN_POINT('Origin',(2.65,2.45,-1.52997821335251));
#8223=CARTESIAN_POINT('Origin',(2.65,0.247141324055048,-1.52997821335251));
#8224=CARTESIAN_POINT('Origin',(1.79136895265445,2.4,-2.02570907967203));
#8225=CARTESIAN_POINT('Origin',(1.79136895265445,2.4,-2.02570907967203));
#8226=CARTESIAN_POINT('Origin',(0.858631047345549,2.4,2.56422556038549));
#8227=CARTESIAN_POINT('Origin',(0.85863104734555,2.4,2.56422556038549));
#8228=CARTESIAN_POINT('Origin',(2.65,0.247141324055048,1.52997821335251));
#8229=CARTESIAN_POINT('Origin',(2.65,0.247141324055048,1.52997821335251));
#8230=CARTESIAN_POINT('Origin',(2.65,0.05,0.538516480713445));
#8231=CARTESIAN_POINT('Origin',(2.65,0.0500000000000002,0.538516480713447));
#8232=CARTESIAN_POINT('Origin',(2.65,0.05,-0.538516480713445));
#8233=CARTESIAN_POINT('Origin',(2.65,0.05,-0.538516480713445));
#8234=CARTESIAN_POINT('Origin',(2.65,0.247141324055048,-1.52997821335251));
#8235=CARTESIAN_POINT('Origin',(2.65,0.247141324055049,-1.52997821335251));
#8236=CARTESIAN_POINT('Origin',(1.325,2.4,-2.29496732002876));
#8237=CARTESIAN_POINT('Origin',(0.858631047345553,2.4,-2.56422556038549));
#8238=CARTESIAN_POINT('Origin',(-1.325,-2.9,2.29496732002876));
#8239=CARTESIAN_POINT('Origin',(2.35402744940532E-17,2.20285867594495,3.05995642670501));
#8240=CARTESIAN_POINT('Origin',(-0.858631047345551,2.4,2.56422556038549));
#8241=CARTESIAN_POINT('Origin',(1.325,-2.9,2.29496732002876));
#8242=CARTESIAN_POINT('Origin',(1.66018457661843E-16,2.20285867594495,3.05995642670502));
#8243=CARTESIAN_POINT('Origin',(1.325,5.35,2.29496732002876));
#8244=CARTESIAN_POINT('Origin',(1.79136895265444,0.0499999999999991,2.02570907967204));
#8245=CARTESIAN_POINT('Origin',(0.,0.0499999999999997,0.));
#8246=CARTESIAN_POINT('Origin',(1.79136895265444,0.05,2.02570907967204));
#8247=CARTESIAN_POINT('Origin',(0.,0.0499999999999997,0.));
#8248=CARTESIAN_POINT('Origin',(1.79136895265444,0.0499999999999996,-2.02570907967204));
#8249=CARTESIAN_POINT('Origin',(1.325,5.35,-2.29496732002876));
#8250=CARTESIAN_POINT('Origin',(1.79136895265444,0.05,-2.02570907967204));
#8251=CARTESIAN_POINT('Origin',(1.325,-2.9,-2.29496732002876));
#8252=CARTESIAN_POINT('Origin',(0.858631047345552,2.4,-2.56422556038549));
#8253=CARTESIAN_POINT('Origin',(6.57489557776427E-16,2.20285867594495,-3.05995642670502));
#8254=CARTESIAN_POINT('Origin',(0.858631047345552,2.4,-2.56422556038549));
#8255=CARTESIAN_POINT('Origin',(0.858631047345552,2.4,-2.56422556038549));
#8256=CARTESIAN_POINT('Origin',(-0.858631047345553,2.4,2.56422556038549));
#8257=CARTESIAN_POINT('Origin',(-0.858631047345553,2.4,2.56422556038549));
#8258=CARTESIAN_POINT('Origin',(5.97981122629482E-17,2.20285867594495,3.05995642670502));
#8259=CARTESIAN_POINT('Origin',(-1.01643953670516E-17,2.20285867594495,
3.05995642670502));
#8260=CARTESIAN_POINT('Origin',(1.79136895265444,0.0499999999999997,2.02570907967204));
#8261=CARTESIAN_POINT('Origin',(1.79136895265444,0.05,2.02570907967204));
#8262=CARTESIAN_POINT('Origin',(1.79136895265444,0.0499999999999999,-2.02570907967204));
#8263=CARTESIAN_POINT('Origin',(1.79136895265444,0.05,-2.02570907967204));
#8264=CARTESIAN_POINT('Origin',(3.69370361905238E-16,2.20285867594495,-3.05995642670502));
#8265=CARTESIAN_POINT('Origin',(-1.01643953670516E-17,2.20285867594495,
-3.05995642670502));
#8266=CARTESIAN_POINT('Origin',(-1.325,-2.9,-2.29496732002876));
#8267=CARTESIAN_POINT('Origin',(-0.85863104734555,2.4,-2.56422556038549));
#8268=CARTESIAN_POINT('Origin',(0.,2.4,0.));
#8269=CARTESIAN_POINT('Origin',(-0.858631047345553,2.4,-2.56422556038549));
#8270=CARTESIAN_POINT('Origin',(0.,2.4,0.));
#8271=CARTESIAN_POINT('Origin',(-1.79136895265445,2.4,2.02570907967203));
#8272=CARTESIAN_POINT('Origin',(-2.65,2.4,0.538516480713457));
#8273=CARTESIAN_POINT('Origin',(-1.325,2.4,2.29496732002876));
#8274=CARTESIAN_POINT('Origin',(-1.79136895265445,2.4,2.02570907967203));
#8275=CARTESIAN_POINT('Origin',(2.16840434497101E-16,2.45,3.05995642670502));
#8276=CARTESIAN_POINT('Origin',(1.55854062294791E-16,0.247141324055048,
3.05995642670502));
#8277=CARTESIAN_POINT('Origin',(1.325,5.35,2.29496732002876));
#8278=CARTESIAN_POINT('Origin',(0.858631047345559,0.05,2.56422556038549));
#8279=CARTESIAN_POINT('Origin',(2.39561377285866E-16,0.247141324055048,
3.05995642670501));
#8280=CARTESIAN_POINT('Origin',(1.325,0.05,2.29496732002876));
#8281=CARTESIAN_POINT('Origin',(0.858631047345558,0.05,2.56422556038549));
#8282=CARTESIAN_POINT('Origin',(1.325,0.05,-2.29496732002876));
#8283=CARTESIAN_POINT('Origin',(0.858631047345559,0.05,-2.56422556038549));
#8284=CARTESIAN_POINT('Origin',(1.325,5.35,-2.29496732002876));
#8285=CARTESIAN_POINT('Origin',(4.60785923306339E-16,0.247141324055048,
-3.05995642670502));
#8286=CARTESIAN_POINT('Origin',(0.858631047345561,0.0500000000000003,-2.56422556038549));
#8287=CARTESIAN_POINT('Origin',(-0.858631047345549,2.4,-2.56422556038549));
#8288=CARTESIAN_POINT('Origin',(-0.858631047345551,2.4,-2.56422556038549));
#8289=CARTESIAN_POINT('Origin',(-2.65,2.4,0.538516480713455));
#8290=CARTESIAN_POINT('Origin',(-2.65,2.4,0.538516480713459));
#8291=CARTESIAN_POINT('Origin',(-2.65,2.4,0.538516480713456));
#8292=CARTESIAN_POINT('Origin',(-1.79136895265445,2.4,2.02570907967203));
#8293=CARTESIAN_POINT('Origin',(-1.79136895265445,2.4,2.02570907967203));
#8294=CARTESIAN_POINT('Origin',(-8.84234197592324E-17,0.247141324055048,
3.05995642670502));
#8295=CARTESIAN_POINT('Origin',(-1.01643953670516E-17,0.247141324055048,
3.05995642670502));
#8296=CARTESIAN_POINT('Origin',(0.858631047345558,0.05,2.56422556038549));
#8297=CARTESIAN_POINT('Origin',(0.858631047345562,0.05,-2.56422556038549));
#8298=CARTESIAN_POINT('Origin',(0.858631047345562,0.05,-2.56422556038549));
#8299=CARTESIAN_POINT('Origin',(4.33176733571846E-16,0.247141324055048,
-3.05995642670502));
#8300=CARTESIAN_POINT('Origin',(5.23648021030599E-16,0.247141324055048,
-3.05995642670501));
#8301=CARTESIAN_POINT('Origin',(-1.325,2.4,-2.29496732002876));
#8302=CARTESIAN_POINT('Origin',(-1.79132934405401,2.40001396671009,-2.02565080655304));
#8303=CARTESIAN_POINT('Origin',(-2.65,2.4,0.));
#8304=CARTESIAN_POINT('Origin',(-2.64992972818517,2.40001396579085,-0.538511314860504));
#8305=CARTESIAN_POINT('Origin',(-2.65,-2.9,0.));
#8306=CARTESIAN_POINT('Origin',(-2.65,2.20285867594495,1.52997821335251));
#8307=CARTESIAN_POINT('Origin',(-1.325,-2.9,2.29496732002876));
#8308=CARTESIAN_POINT('Origin',(-2.65,2.20285867594495,1.52997821335251));
#8309=CARTESIAN_POINT('Origin',(-1.325,5.35,2.29496732002876));
#8310=CARTESIAN_POINT('Origin',(-0.858631047345555,0.0499999999999995,2.56422556038549));
#8311=CARTESIAN_POINT('Origin',(0.,0.0499999999999997,0.));
#8312=CARTESIAN_POINT('Origin',(-0.858631047345555,0.0499999999999992,-2.56422556038549));
#8313=CARTESIAN_POINT('Origin',(-1.325,5.35,-2.29496732002876));
#8314=CARTESIAN_POINT('Origin',(-0.858631047345559,0.05,-2.56422556038549));
#8315=CARTESIAN_POINT('Origin',(-1.325,-2.9,-2.29496732002876));
#8316=CARTESIAN_POINT('Origin',(-2.65,2.20285867594495,-1.52997821335251));
#8317=CARTESIAN_POINT('Origin',(-2.65,-2.9,0.));
#8318=CARTESIAN_POINT('Origin',(-2.65,2.20285867594495,-1.52997821335251));
#8319=CARTESIAN_POINT('Origin',(-2.65,2.20285867594495,1.52997821335251));
#8320=CARTESIAN_POINT('Origin',(-2.65,2.20285867594495,1.52997821335251));
#8321=CARTESIAN_POINT('Origin',(-0.858631047345559,0.05,2.56422556038549));
#8322=CARTESIAN_POINT('Origin',(-0.858631047345559,0.05,2.56422556038549));
#8323=CARTESIAN_POINT('Origin',(-0.858631047345557,0.0499999999999997,-2.56422556038549));
#8324=CARTESIAN_POINT('Origin',(-0.858631047345558,0.05,-2.56422556038549));
#8325=CARTESIAN_POINT('Origin',(-2.65,2.20285867594495,-1.52997821335251));
#8326=CARTESIAN_POINT('Origin',(-2.65,2.20285867594495,-1.52997821335251));
#8327=CARTESIAN_POINT('Origin',(-2.65,2.45,1.52997821335251));
#8328=CARTESIAN_POINT('Origin',(-2.65,0.247141324055048,1.52997821335251));
#8329=CARTESIAN_POINT('Origin',(-1.325,5.35,2.29496732002876));
#8330=CARTESIAN_POINT('Origin',(-1.79136895265444,0.05,2.02570907967204));
#8331=CARTESIAN_POINT('Origin',(-2.65,0.247141324055048,1.52997821335251));
#8332=CARTESIAN_POINT('Origin',(-1.325,0.05,2.29496732002876));
#8333=CARTESIAN_POINT('Origin',(-1.79136895265444,0.05,2.02570907967204));
#8334=CARTESIAN_POINT('Origin',(-1.325,0.05,-2.29496732002876));
#8335=CARTESIAN_POINT('Origin',(-1.79136895265444,0.05,-2.02570907967204));
#8336=CARTESIAN_POINT('Origin',(-1.325,5.35,-2.29496732002876));
#8337=CARTESIAN_POINT('Origin',(-2.65,0.247141324055048,-1.52997821335251));
#8338=CARTESIAN_POINT('Origin',(-1.79136895265444,0.0499999999999991,-2.02570907967204));
#8339=CARTESIAN_POINT('Origin',(-2.65,2.45,-1.52997821335251));
#8340=CARTESIAN_POINT('Origin',(-2.65,0.247141324055048,-1.52997821335251));
#8341=CARTESIAN_POINT('Origin',(-2.65,0.247141324055048,1.52997821335251));
#8342=CARTESIAN_POINT('Origin',(-2.65,0.247141324055048,1.52997821335251));
#8343=CARTESIAN_POINT('Origin',(-1.79136895265444,0.05,2.02570907967204));
#8344=CARTESIAN_POINT('Origin',(-1.79136895265444,0.0500000000000002,2.02570907967204));
#8345=CARTESIAN_POINT('Origin',(-1.79136895265444,0.0499999999999997,-2.02570907967204));
#8346=CARTESIAN_POINT('Origin',(-1.79136895265444,0.05,-2.02570907967204));
#8347=CARTESIAN_POINT('Origin',(-2.65,0.247141324055048,-1.52997821335251));
#8348=CARTESIAN_POINT('Origin',(-2.65,0.247141324055048,-1.52997821335251));
#8349=CARTESIAN_POINT('Origin',(-2.65,5.35,0.));
#8350=CARTESIAN_POINT('Origin',(-2.65,0.0500000000000003,0.538516480713448));
#8351=CARTESIAN_POINT('Origin',(0.,0.0499999999999997,0.));
#8352=CARTESIAN_POINT('Origin',(-2.65,0.05,0.538516480713445));
#8353=CARTESIAN_POINT('Origin',(0.,0.0499999999999997,0.));
#8354=CARTESIAN_POINT('Origin',(-2.65,0.0500000000000001,-0.538516480713447));
#8355=CARTESIAN_POINT('Origin',(-2.65,5.35,0.));
#8356=CARTESIAN_POINT('Origin',(-2.65,0.05,-0.538516480713451));
#8357=CARTESIAN_POINT('Origin',(-2.65,0.05,0.538516480713445));
#8358=CARTESIAN_POINT('Origin',(-2.65,0.05,0.538516480713451));
#8359=CARTESIAN_POINT('Origin',(-2.65,0.05,-0.538516480713445));
#8360=CARTESIAN_POINT('Origin',(-2.65,0.05,-0.538516480713445));
#8361=CARTESIAN_POINT('Origin',(-2.65,0.05,0.));
#8362=CARTESIAN_POINT('Origin',(0.,4.85,0.));
#8363=CARTESIAN_POINT('',(0.,0.,0.));
#8364=CARTESIAN_POINT('Origin',(0.,0.,0.));
#8365=CARTESIAN_POINT('',(-1.83697019872103E-16,-1.22464679914735E-16,1.5));
#8366=CARTESIAN_POINT('Origin',(-3.06161699786838E-16,0.,2.5));
#8367=CARTESIAN_POINT('Origin',(0.,1.22464679914735E-16,0.));
#8368=CARTESIAN_POINT('',(0.,0.,0.));
#8369=CARTESIAN_POINT('Origin',(0.,0.,0.));
#8370=CARTESIAN_POINT('',(-6.58247654541702E-16,-2.14313189850787E-17,5.375));
#8371=CARTESIAN_POINT('Origin',(-6.79678973526781E-16,0.,5.55));
#8372=CARTESIAN_POINT('Origin',(0.,2.14313189850787E-17,0.));
#8373=CARTESIAN_POINT('Origin',(0.,11.,0.));
#8374=CARTESIAN_POINT('',(-3.67484018169097E-16,11.,3.00073472959676));
#8375=CARTESIAN_POINT('Origin',(-3.88915337154176E-16,11.,3.17573472959676));
#8376=CARTESIAN_POINT('Origin',(0.,11.,0.));
#8377=CARTESIAN_POINT('',(-2.3674783363584,10.9996616868026,-2.37117425835928));
#8378=CARTESIAN_POINT('',(-2.36654172903753,11.0369221330747,-2.36654172907039));
#8379=CARTESIAN_POINT('Ctrl Pts',(-2.36654172902905,11.0369221332381,-2.36654172902901));
#8380=CARTESIAN_POINT('Ctrl Pts',(-2.36660261520315,11.0363244725787,-2.36666327705626));
#8381=CARTESIAN_POINT('Ctrl Pts',(-2.36666128562436,11.0357261397191,-2.36678260888203));
#8382=CARTESIAN_POINT('Ctrl Pts',(-2.36723393352068,11.029650121596,-2.36797057219123));
#8383=CARTESIAN_POINT('Ctrl Pts',(-2.36756434090361,11.0241223710425,-2.36885504265911));
#8384=CARTESIAN_POINT('Ctrl Pts',(-2.36786981099157,11.0122851763974,-2.37033490110904));
#8385=CARTESIAN_POINT('Ctrl Pts',(-2.36779322640185,11.0059755411538,-2.37087710768974));
#8386=CARTESIAN_POINT('Ctrl Pts',(-2.36747833635822,10.9996616867988,-2.37117425835944));
#8387=CARTESIAN_POINT('',(-2.45534485149915,10.9282219455009,-1.7516666854678));
#8388=CARTESIAN_POINT('Ctrl Pts',(-2.36654172902905,11.0369221332381,-2.36654172902902));
#8389=CARTESIAN_POINT('Ctrl Pts',(-2.37334411896229,11.0362823302019,-2.35993463713669));
#8390=CARTESIAN_POINT('Ctrl Pts',(-2.38011577585649,11.0356428039708,-2.35329589463348));
#8391=CARTESIAN_POINT('Ctrl Pts',(-2.54314617762233,11.0201812306806,-2.19197276001336));
#8392=CARTESIAN_POINT('Ctrl Pts',(-2.68269334753296,11.0055217449001,-2.0205521909063));
#8393=CARTESIAN_POINT('Ctrl Pts',(-2.93077377794738,10.9744992833803,-1.63885953638735));
#8394=CARTESIAN_POINT('Ctrl Pts',(-3.03643612092201,10.9580589959793,-1.42666947885773));
#8395=CARTESIAN_POINT('Ctrl Pts',(-3.24828372828744,10.9112686417533,-0.832197869920266));
#8396=CARTESIAN_POINT('Ctrl Pts',(-3.28050325458791,10.8850718442332,-0.503072235115654));
#8397=CARTESIAN_POINT('Ctrl Pts',(-3.27116719523908,10.8542407041749,-0.173247696238549));
#8398=CARTESIAN_POINT('Ctrl Pts',(-3.25839405608137,10.8451986333149,-0.0885221583575347));
#8399=CARTESIAN_POINT('Ctrl Pts',(-3.23881660723628,10.8367580084259,-0.0305206064263497));
#8400=CARTESIAN_POINT('Ctrl Pts',(-3.23350366077321,10.8346759734772,-0.0174528173977804));
#8401=CARTESIAN_POINT('Ctrl Pts',(-3.22490854320742,10.8320397599134,-0.00643610865276417));
#8402=CARTESIAN_POINT('Ctrl Pts',(-3.22255570142893,10.8313575488208,-0.00396872044824001));
#8403=CARTESIAN_POINT('Ctrl Pts',(-3.21825792744808,10.8302367058123,-0.00122700918978464));
#8404=CARTESIAN_POINT('Ctrl Pts',(-3.21649608927482,10.8298022464972,-0.000455877488832637));
#8405=CARTESIAN_POINT('Ctrl Pts',(-3.21302387578014,10.8290112656581,0.000142774382210926));
#8406=CARTESIAN_POINT('Ctrl Pts',(-3.21144786498889,10.828675339728,8.85061552719118E-5));
#8407=CARTESIAN_POINT('Ctrl Pts',(-3.20813643512089,10.8280166434058,-0.000687603043136314));
#8408=CARTESIAN_POINT('Ctrl Pts',(-3.2065013980317,10.8277189617055,-0.00145760483001095));
#8409=CARTESIAN_POINT('Ctrl Pts',(-3.20251334962923,10.8270431196483,-0.00403322970158444));
#8410=CARTESIAN_POINT('Ctrl Pts',(-3.20028633028751,10.8267209281034,-0.00623711459830585));
#8411=CARTESIAN_POINT('Ctrl Pts',(-3.19410520074952,10.8259164744266,-0.0135679320571353));
#8412=CARTESIAN_POINT('Ctrl Pts',(-3.19023496381139,10.8255747732312,-0.0203458579147062));
#8413=CARTESIAN_POINT('Ctrl Pts',(-3.1768815605095,10.8247309008079,-0.0479485545610701));
#8414=CARTESIAN_POINT('Ctrl Pts',(-3.16735042929677,10.8249800714079,-0.0783448786336477));
#8415=CARTESIAN_POINT('Ctrl Pts',(-3.11478686213639,10.8290765772632,-0.269802373389443));
#8416=CARTESIAN_POINT('Ctrl Pts',(-3.06060090440076,10.843895246432,-0.566826036283537));
#8417=CARTESIAN_POINT('Ctrl Pts',(-2.86004093617191,10.876114649494,-1.07584184708214));
#8418=CARTESIAN_POINT('Ctrl Pts',(-2.78959762400602,10.8863469276679,-1.22442516795858));
#8419=CARTESIAN_POINT('Ctrl Pts',(-2.66904925825053,10.9023565788694,-1.43719223473247));
#8420=CARTESIAN_POINT('Ctrl Pts',(-2.62779792624269,10.9076260262076,-1.50448086866193));
#8421=CARTESIAN_POINT('Ctrl Pts',(-2.5432634370422,10.917999580532,-1.63214960111092));
#8422=CARTESIAN_POINT('Ctrl Pts',(-2.50029161260727,10.9230894885434,-1.69263839311565));
#8423=CARTESIAN_POINT('Ctrl Pts',(-2.45534485149905,10.9282219455009,-1.75166668546793));
#8424=CARTESIAN_POINT('',(-2.12462539575998,10.9630778666627,-2.12462539640225));
#8425=CARTESIAN_POINT('Ctrl Pts',(-2.45534485149915,10.9282219455009,-1.7516666854678));
#8426=CARTESIAN_POINT('Ctrl Pts',(-2.40908054625928,10.9335048524215,-1.81242530005626));
#8427=CARTESIAN_POINT('Ctrl Pts',(-2.3606379133253,10.9388413422232,-1.87174235306124));
#8428=CARTESIAN_POINT('Ctrl Pts',(-2.31017054130683,10.9442027102673,-1.92935832892452));
#8429=CARTESIAN_POINT('Ctrl Pts',(-2.26186164921788,10.949334773617,-1.98451008042768));
#8430=CARTESIAN_POINT('Ctrl Pts',(-2.21169772289672,10.9544892409942,-2.03810240827354));
#8431=CARTESIAN_POINT('Ctrl Pts',(-2.15984481067586,10.9596213484018,-2.08993852779845));
#8432=CARTESIAN_POINT('Ctrl Pts',(-2.14818952039214,10.960774922985,-2.10159004348713));
#8433=CARTESIAN_POINT('Ctrl Pts',(-2.13644901713658,10.9619273010852,-2.11315298186845));
#8434=CARTESIAN_POINT('Ctrl Pts',(-2.12462539575998,10.9630778666627,-2.12462539640225));
#8435=CARTESIAN_POINT('Origin',(-2.24558440890951,11.0000054639071,-2.24558417873147));
#8436=CARTESIAN_POINT('Ctrl Pts',(-2.36456791311707,11.0001838839337,-2.37391751282759));
#8437=CARTESIAN_POINT('Ctrl Pts',(-2.68439695740737,10.9428309226217,-2.07282384920463));
#8438=CARTESIAN_POINT('Ctrl Pts',(-2.94593475213736,10.885477961311,-1.70638527343931));
#8439=CARTESIAN_POINT('Ctrl Pts',(-3.30964371429254,10.7708333333336,-0.896538039613314));
#8440=CARTESIAN_POINT('Ctrl Pts',(-3.41180604852602,10.7135416666669,-0.453515668913589));
#8441=CARTESIAN_POINT('Ctrl Pts',(-3.4379002366457,10.5989583333331,0.443108774718904));
#8442=CARTESIAN_POINT('Ctrl Pts',(-3.36178304590245,10.5416666666666,0.896358100460257));
#8443=CARTESIAN_POINT('Ctrl Pts',(-3.03905091217473,10.4270833333334,1.74368979436799));
#8444=CARTESIAN_POINT('Ctrl Pts',(-2.79252711081109,10.3697916666664,2.13742396723561));
#8445=CARTESIAN_POINT('Ctrl Pts',(-2.16323413009096,10.2552083333337,2.80361970275416));
#8446=CARTESIAN_POINT('Ctrl Pts',(-1.78068510549046,10.1979166666664,3.07579175088966));
#8447=CARTESIAN_POINT('Ctrl Pts',(-0.935379221363662,10.0833333333336,3.45417305821104));
#8448=CARTESIAN_POINT('Ctrl Pts',(-0.472940081479242,10.0260416666666,3.56019762788479));
#8449=CARTESIAN_POINT('Ctrl Pts',(0.462533187284589,9.91145833333345,3.58629181608734));
#8450=CARTESIAN_POINT('Ctrl Pts',(0.935199282188079,9.85416666666669,3.50631238974053));
#8451=CARTESIAN_POINT('Ctrl Pts',(1.81842261051809,9.73958333333332,3.16871345434639));
#8452=CARTESIAN_POINT('Ctrl Pts',(2.22861752543397,9.68229166666673,2.91119093668731));
#8453=CARTESIAN_POINT('Ctrl Pts',(2.92228352868554,9.56770833333328,2.25442768834444));
#8454=CARTESIAN_POINT('Ctrl Pts',(3.20545429299277,9.51041666666666,1.85541792160244));
#8455=CARTESIAN_POINT('Ctrl Pts',(3.59870240211769,9.39583333333334,0.974220403129539));
#8456=CARTESIAN_POINT('Ctrl Pts',(3.70858920724845,9.3385416666664,0.492364494026195));
#8457=CARTESIAN_POINT('Ctrl Pts',(3.73468339552408,9.22395833333361,-0.481957599831572));
#8458=CARTESIAN_POINT('Ctrl Pts',(3.65084173357628,9.16666666666689,-0.974040463933888));
#8459=CARTESIAN_POINT('Ctrl Pts',(3.29837599652037,9.05208333333312,-1.8931554266502));
#8460=CARTESIAN_POINT('Ctrl Pts',(3.02985476255422,8.99479166666641,-2.31981108364774));
#8461=CARTESIAN_POINT('Ctrl Pts',(2.34562124660724,8.8802083333336,-3.04094735460153));
#8462=CARTESIAN_POINT('Ctrl Pts',(1.93015073770027,8.82291666666647,-3.33511683510577));
#8463=CARTESIAN_POINT('Ctrl Pts',(1.01306158490958,8.70833333333354,-3.74323174601444));
#8464=CARTESIAN_POINT('Ctrl Pts',(0.511788906557484,8.6510416666665,-3.85698078661577));
#8465=CARTESIAN_POINT('Ctrl Pts',(-0.501382012362897,8.53645833333351,-3.88307497495716));
#8466=CARTESIAN_POINT('Ctrl Pts',(-1.01288164569554,8.47916666666683,-3.79537107740945));
#8467=CARTESIAN_POINT('Ctrl Pts',(-1.96788824276646,8.36458333333318,-3.42803853869692));
#8468=CARTESIAN_POINT('Ctrl Pts',(-2.41100464187403,8.30729166666683,-3.14851858841386));
#8469=CARTESIAN_POINT('Ctrl Pts',(-3.159611180505,8.1927083333332,-2.43681480487731));
#8470=CARTESIAN_POINT('Ctrl Pts',(-3.46477937722837,8.13541666666656,-2.00488355378617));
#8471=CARTESIAN_POINT('Ctrl Pts',(-3.8877610899016,8.02083333333345,-1.05190276670153));
#8472=CARTESIAN_POINT('Ctrl Pts',(-4.00537236598643,7.96354166666637,-0.531213319073915));
#8473=CARTESIAN_POINT('Ctrl Pts',(-4.03146655438691,7.84895833333365,0.520806424879362));
#8474=CARTESIAN_POINT('Ctrl Pts',(-3.93990042124014,7.79166666666665,1.05172282747159));
#8475=CARTESIAN_POINT('Ctrl Pts',(-3.55770108087595,7.67708333333337,2.04262105886835));
#8476=CARTESIAN_POINT('Ctrl Pts',(-3.26718241426475,7.61979166666659,2.50219820011361));
#8477=CARTESIAN_POINT('Ctrl Pts',(-2.52800836315612,7.50520833333343,3.27827500639517));
#8478=CARTESIAN_POINT('Ctrl Pts',(-2.07961636986072,7.44791666666668,3.59444191935829));
#8479=CARTESIAN_POINT('Ctrl Pts',(-1.09074394850484,7.33333333333333,4.03229043378143));
#8480=CARTESIAN_POINT('Ctrl Pts',(-0.550637731576509,7.27604166666629,4.15376394536062));
#8481=CARTESIAN_POINT('Ctrl Pts',(0.540230837381994,7.16145833333372,4.17985813381312));
#8482=CARTESIAN_POINT('Ctrl Pts',(1.09056400926098,7.10416666666678,4.08442976506864));
#8483=CARTESIAN_POINT('Ctrl Pts',(2.11735387495688,6.98958333333323,3.68736362305719));
#8484=CARTESIAN_POINT('Ctrl Pts',(2.59339175836345,6.93229166666724,3.38584624010982));
#8485=CARTESIAN_POINT('Ctrl Pts',(3.3969388322751,6.81770833333277,2.61920192144075));
#8486=CARTESIAN_POINT('Ctrl Pts',(3.72410446149635,6.76041666666712,2.15434918592434));
#8487=CARTESIAN_POINT('Ctrl Pts',(4.17681977765313,6.64583333333289,1.12958513031907));
#8488=CARTESIAN_POINT('Ctrl Pts',(4.30215552473732,6.58854166666688,0.570062144068889));
#8489=CARTESIAN_POINT('Ctrl Pts',(4.32824971323683,6.47395833333313,-0.559655249874413));
#8490=CARTESIAN_POINT('Ctrl Pts',(4.22895910889563,6.41666666666645,-1.12940519106012));
#8491=CARTESIAN_POINT('Ctrl Pts',(3.81702616523991,6.30208333333356,-2.19208669103568));
#8492=CARTESIAN_POINT('Ctrl Pts',(3.50451006594675,6.24479166666656,-2.68458531662391));
#8493=CARTESIAN_POINT('Ctrl Pts',(2.71039547973352,6.13020833333345,-3.51560265814439));
#8494=CARTESIAN_POINT('Ctrl Pts',(2.22908200197935,6.07291666666717,-3.85376700363998));
#8495=CARTESIAN_POINT('Ctrl Pts',(1.16842631214193,5.95833333333284,-4.32134912151925));
#8496=CARTESIAN_POINT('Ctrl Pts',(0.589486556547344,5.90104166666655,-4.45054710411593));
#8497=CARTESIAN_POINT('Ctrl Pts',(-0.579079662352908,5.78645833333346,-4.47664129265863));
#8498=CARTESIAN_POINT('Ctrl Pts',(-1.16824637287424,5.72916666666705,-4.37348845271886));
#8499=CARTESIAN_POINT('Ctrl Pts',(-2.26681950709949,5.61458333333296,-3.94668870742641));
#8500=CARTESIAN_POINT('Ctrl Pts',(-2.77577887489086,5.55729166666709,-3.62317389178086));
#8501=CARTESIAN_POINT('Ctrl Pts',(-3.6342664840072,5.44270833333292,-2.80158903802911));
#8502=CARTESIAN_POINT('Ctrl Pts',(-3.98342954578962,5.38541666666669,-2.30381481802579));
#8503=CARTESIAN_POINT('Ctrl Pts',(-4.46587846537937,5.27083333333332,-1.20726749397333));
#8504=CARTESIAN_POINT('Ctrl Pts',(-4.59893868349712,5.21354166666665,-0.608910969019916));
#8505=CARTESIAN_POINT('Ctrl Pts',(-4.62503287207784,5.09895833333335,0.598504074825539));
#8506=CARTESIAN_POINT('Ctrl Pts',(-4.51801779654147,5.04166666666663,1.20708755469526));
#8507=CARTESIAN_POINT('Ctrl Pts',(-4.07635124961353,4.92708333333338,2.34155232315641));
#8508=CARTESIAN_POINT('Ctrl Pts',(-3.74183771760646,4.86979166666659,2.86697243316876));
#8509=CARTESIAN_POINT('Ctrl Pts',(-2.89278259633321,4.75520833333342,3.75293030985906));
#8510=CARTESIAN_POINT('Ctrl Pts',(-2.37854763406351,4.69791666666658,4.1130920879442));
#8511=CARTESIAN_POINT('Ctrl Pts',(-1.24610867581347,4.58333333333343,4.61040780923455));
#8512=CARTESIAN_POINT('Ctrl Pts',(-0.628335381481812,4.52604166666658,4.74733026287932));
#8513=CARTESIAN_POINT('Ctrl Pts',(0.617928487287482,4.41145833333343,4.77342445149605));
#8514=CARTESIAN_POINT('Ctrl Pts',(1.24592873652376,4.35416666666679,4.66254714036264));
#8515=CARTESIAN_POINT('Ctrl Pts',(2.41628513920584,4.23958333333322,4.20601379180208));
#8516=CARTESIAN_POINT('Ctrl Pts',(2.95816599145146,4.18229166666676,3.86050154342994));
#8517=CARTESIAN_POINT('Ctrl Pts',(3.87159413570613,4.06770833333325,2.98397615463943));
#8518=CARTESIAN_POINT('Ctrl Pts',(4.24275463010319,4.01041666666671,2.45328045009706));
#8519=CARTESIAN_POINT('Ctrl Pts',(4.75493715308532,3.8958333333333,1.28494985765777));
#8520=CARTESIAN_POINT('Ctrl Pts',(4.89572184226387,3.83854166666642,0.647759793932574));
#8521=CARTESIAN_POINT('Ctrl Pts',(4.9218160309119,3.72395833333359,-0.637352899738291));
#8522=CARTESIAN_POINT('Ctrl Pts',(4.80707648417982,3.66666666666662,-1.28476991836542));
#8523=CARTESIAN_POINT('Ctrl Pts',(4.33567633399462,3.55208333333339,-2.49101795524214));
#8524=CARTESIAN_POINT('Ctrl Pts',(3.97916536924807,3.49479166666671,-3.04935954974168));
#8525=CARTESIAN_POINT('Ctrl Pts',(3.075169712951,3.38020833333329,-3.99025796154567));
#8526=CARTESIAN_POINT('Ctrl Pts',(2.52801326612096,3.3229166666668,-4.37241717226731));
#8527=CARTESIAN_POINT('Ctrl Pts',(1.3237910395117,3.20833333333321,-4.89946649693097));
#8528=CARTESIAN_POINT('Ctrl Pts',(0.667184206381905,3.15104166666636,-5.04411342164931));
#8529=CARTESIAN_POINT('Ctrl Pts',(-0.656777312187654,3.03645833333365,-5.07020761032686));
#8530=CARTESIAN_POINT('Ctrl Pts',(-1.32361110020785,2.97916666666654,-4.95160582799841));
#8531=CARTESIAN_POINT('Ctrl Pts',(-2.56575077127763,2.86458333333347,-4.46533887618575));
#8532=CARTESIAN_POINT('Ctrl Pts',(-3.1405531080382,2.80729166666695,-4.09782919506089));
#8533=CARTESIAN_POINT('Ctrl Pts',(-4.10892178737893,2.69270833333305,-3.16636327126786));
#8534=CARTESIAN_POINT('Ctrl Pts',(-4.50207971443576,2.63541666666658,-2.60274608213879));
#8535=CARTESIAN_POINT('Ctrl Pts',(-5.04399584077227,2.52083333333343,-1.36263222137173));
#8536=CARTESIAN_POINT('Ctrl Pts',(-5.1925050010359,2.4635416666663,-0.686608618821642));
#8537=CARTESIAN_POINT('Ctrl Pts',(-5.21859918974068,2.34895833333371,0.67620172462746));
#8538=CARTESIAN_POINT('Ctrl Pts',(-5.09613517181383,2.29166666666676,1.36245228206106));
#8539=CARTESIAN_POINT('Ctrl Pts',(-4.59500141838005,2.17708333333325,2.64048358730238));
#8540=CARTESIAN_POINT('Ctrl Pts',(-4.21649302087059,2.11979166666664,3.23174666634004));
#8541=CARTESIAN_POINT('Ctrl Pts',(-3.25755682958786,2.00520833333337,4.22758561320685));
#8542=CARTESIAN_POINT('Ctrl Pts',(-2.67747889815098,1.94791666666658,4.63174225660692));
#8543=CARTESIAN_POINT('Ctrl Pts',(-1.40147340323737,1.83333333333343,5.18852518461089));
#8544=CARTESIAN_POINT('Ctrl Pts',(-0.706033031254986,1.77604166666627,5.34089658042353));
#8545=CARTESIAN_POINT('Ctrl Pts',(0.695626137060878,1.66145833333374,5.36699076915345));
#8546=CARTESIAN_POINT('Ctrl Pts',(1.40129346391331,1.60416666666663,5.24066451563091));
#8547=CARTESIAN_POINT('Ctrl Pts',(2.71521640332806,1.48958333333338,4.7246639605727));
#8548=CARTESIAN_POINT('Ctrl Pts',(3.32294022464786,1.43229166666683,4.33515684667557));
#8549=CARTESIAN_POINT('Ctrl Pts',(4.34624943902881,1.31770833333318,3.34875038791256));
#8550=CARTESIAN_POINT('Ctrl Pts',(4.76140479878007,1.26041666666641,2.75221171416214));
#8551=CARTESIAN_POINT('Ctrl Pts',(5.3330545284475,1.1458333333336,1.44031458510402));
#8552=CARTESIAN_POINT('Ctrl Pts',(5.48928815981245,1.08854166666688,0.72545744367903));
#8553=CARTESIAN_POINT('Ctrl Pts',(5.51538234856494,0.973958333333134,-0.715050549484959));
#8554=CARTESIAN_POINT('Ctrl Pts',(5.38519385944284,0.916666666666909,-1.44013464577813));
#8555=CARTESIAN_POINT('Ctrl Pts',(4.85432650277048,0.8020833333331,-2.7899492193412));
#8556=CARTESIAN_POINT('Ctrl Pts',(4.4538206724838,0.744791666666392,-3.4141337829535));
#8557=CARTESIAN_POINT('Ctrl Pts',(3.43994394623404,0.630208333333619,-4.46491326485293));
#8558=CARTESIAN_POINT('Ctrl Pts',(2.82694453016243,0.572916666666411,-4.89106734095877));
#8559=CARTESIAN_POINT('Ctrl Pts',(1.47915576698159,0.4583333333336,-5.47758387227856));
#8560=CARTESIAN_POINT('Ctrl Pts',(0.744881856102772,0.401041666666677,-5.63767973920226));
#8561=CARTESIAN_POINT('Ctrl Pts',(-0.73447496190878,0.286458333333334,-5.66377392797554));
#8562=CARTESIAN_POINT('Ctrl Pts',(-1.4789758276525,0.229166666666838,-5.52972320325324));
#8563=CARTESIAN_POINT('Ctrl Pts',(-2.86468203534475,0.114583333333173,-4.9839890449698));
#8564=CARTESIAN_POINT('Ctrl Pts',(-3.50532733285514,0.0572916666665569,
-4.5724845058884));
#8565=CARTESIAN_POINT('Ctrl Pts',(-4.04445221596811,5.20417042793042E-15,
-4.05181100142375));
#8566=CARTESIAN_POINT('Ctrl Pts',(-2.39934536183762,11.346909399206,-2.34117692464435));
#8567=CARTESIAN_POINT('Ctrl Pts',(-2.71488410852275,11.2895564378939,-2.03552600632456));
#8568=CARTESIAN_POINT('Ctrl Pts',(-2.9712261341221,11.2322034765833,-1.66538602697384));
#8569=CARTESIAN_POINT('Ctrl Pts',(-3.32352361490692,11.1175588486058,-0.850409340498224));
#8570=CARTESIAN_POINT('Ctrl Pts',(-3.4194758201212,11.0602671819391,-0.405958512493029));
#8571=CARTESIAN_POINT('Ctrl Pts',(-3.43307090382695,10.9456838486053,0.491037743700738));
#8572=CARTESIAN_POINT('Ctrl Pts',(-3.35066965504748,10.8883921819389,0.943230278421825));
#8573=CARTESIAN_POINT('Ctrl Pts',(-3.01624756806638,10.7738088486056,1.78612228216488));
#8574=CARTESIAN_POINT('Ctrl Pts',(-2.76432247051982,10.7165171819386,2.17647530254211));
#8575=CARTESIAN_POINT('Ctrl Pts',(-2.12592837712132,10.6019338486059,2.83409574774927));
#8576=CARTESIAN_POINT('Ctrl Pts',(-1.7396831165707,10.5446421819387,3.10107703174287));
#8577=CARTESIAN_POINT('Ctrl Pts',(-0.889250522245734,10.4300588486058,3.46805295881896));
#8578=CARTESIAN_POINT('Ctrl Pts',(-0.425382925058827,10.3727671819388,3.56786739948684));
#8579=CARTESIAN_POINT('Ctrl Pts',(0.510462156266568,10.2581838486057,3.58146248326171));
#8580=CARTESIAN_POINT('Ctrl Pts',(0.982071460151994,10.2008921819389,3.49519899889172));
#8581=CARTESIAN_POINT('Ctrl Pts',(1.86085509831263,10.0863088486056,3.14591011023186));
#8582=CARTESIAN_POINT('Ctrl Pts',(2.26766886074488,10.029017181939,2.88298629640079));
#8583=CARTESIAN_POINT('Ctrl Pts',(2.95275957367625,9.91443384860552,2.21712193537007));
#8584=CARTESIAN_POINT('Ctrl Pts',(3.2307395738517,9.8571421819389,1.81441593268519));
#8585=CARTESIAN_POINT('Ctrl Pts',(3.61258230271989,9.74255884860558,0.9280917040091));
#8586=CARTESIAN_POINT('Ctrl Pts',(3.71625897885657,9.68526718193864,0.444807337606009));
#8587=CARTESIAN_POINT('Ctrl Pts',(3.72985406269238,9.57068384860585,-0.52988656881378));
#8588=CARTESIAN_POINT('Ctrl Pts',(3.63972834273301,9.51339218193913,-1.02091264189992));
#8589=CARTESIAN_POINT('Ctrl Pts',(3.2755726524003,9.39880884860535,-1.93558791444263));
#8590=CARTESIAN_POINT('Ctrl Pts',(3.00165012227183,9.34151718193865,-2.35886241896257));
#8591=CARTESIAN_POINT('Ctrl Pts',(2.30831549362873,9.22693384860584,-3.07142339958832));
#8592=CARTESIAN_POINT('Ctrl Pts',(1.88914874878537,9.1696421819387,-3.3604021159697));
#8593=CARTESIAN_POINT('Ctrl Pts',(0.966932885786784,9.05505884860578,-3.75711164661164));
#8594=CARTESIAN_POINT('Ctrl Pts',(0.46423175013744,8.99776718193874,-3.86465055822945));
#8595=CARTESIAN_POINT('Ctrl Pts',(-0.549310981345248,8.88318384860575,-3.87824564211992));
#8596=CARTESIAN_POINT('Ctrl Pts',(-1.05975382366345,8.82589218193907,-3.78425768657106));
#8597=CARTESIAN_POINT('Ctrl Pts',(-2.01032073055702,8.71130884860541,-3.40523519457197));
#8598=CARTESIAN_POINT('Ctrl Pts',(-2.45005597719243,8.65401718193906,-3.12031394813519));
#8599=CARTESIAN_POINT('Ctrl Pts',(-3.19008722548821,8.53943384860543,-2.39950905189507));
#8600=CARTESIAN_POINT('Ctrl Pts',(-3.49006465809683,8.4821421819388,-1.96388156487328));
#8601=CARTESIAN_POINT('Ctrl Pts',(-3.90164099049427,8.36755884860569,-1.00577406757673));
#8602=CARTESIAN_POINT('Ctrl Pts',(-4.01304213760465,8.3102671819386,-0.483656162654029));
#8603=CARTESIAN_POINT('Ctrl Pts',(-4.02663722154512,8.19568384860588,0.568735393861871));
#8604=CARTESIAN_POINT('Ctrl Pts',(-3.92878703040616,8.13839218193865,1.09859500544122));
#8605=CARTESIAN_POINT('Ctrl Pts',(-3.5348977367466,8.02380884860583,2.08505354665718));
#8606=CARTESIAN_POINT('Ctrl Pts',(-3.23897777398945,7.96651718193906,2.54124953543508));
#8607=CARTESIAN_POINT('Ctrl Pts',(-2.49070261017052,7.85193384860543,3.30875105137532));
#8608=CARTESIAN_POINT('Ctrl Pts',(-2.03861438094966,7.79464218193892,3.61972720023077));
#8609=CARTESIAN_POINT('Ctrl Pts',(-1.0446152493782,7.68005884860556,4.04617033437007));
#8610=CARTESIAN_POINT('Ctrl Pts',(-0.503080575156725,7.62276718193853,4.16143371698328));
#8611=CARTESIAN_POINT('Ctrl Pts',(0.588159806364604,7.50818384860596,4.17502880096689));
#8612=CARTESIAN_POINT('Ctrl Pts',(1.13743618723204,7.45089218193902,4.07331637423875));
#8613=CARTESIAN_POINT('Ctrl Pts',(2.15978636274428,7.33630884860546,3.66456027892374));
#8614=CARTESIAN_POINT('Ctrl Pts',(2.63244309368768,7.27901718193947,3.35764159983753));
#8615=CARTESIAN_POINT('Ctrl Pts',(3.42741487725249,7.16443384860501,2.58189616845213));
#8616=CARTESIAN_POINT('Ctrl Pts',(3.74938974237272,7.10714218193936,2.11334719701498));
#8617=CARTESIAN_POINT('Ctrl Pts',(4.19069967823789,6.99255884860513,1.08345643119075));
#8618=CARTESIAN_POINT('Ctrl Pts',(4.30982529636403,6.93526718193912,0.522504987649244));
#8619=CARTESIAN_POINT('Ctrl Pts',(4.32342038038655,6.82068384860537,-0.607584218857162));
#8620=CARTESIAN_POINT('Ctrl Pts',(4.21784571806929,6.76339218193869,-1.17627736903264));
#8621=CARTESIAN_POINT('Ctrl Pts',(3.79422282110293,6.6488088486058,-2.23451917882162));
#8622=CARTESIAN_POINT('Ctrl Pts',(3.47630542567715,6.5915171819388,-2.72363665195073));
#8623=CARTESIAN_POINT('Ctrl Pts',(2.67308972674222,6.47693384860569,-3.54607870311919));
#8624=CARTESIAN_POINT('Ctrl Pts',(2.18808001307138,6.41964218193941,-3.87905228451955));
#8625=CARTESIAN_POINT('Ctrl Pts',(1.1222976130122,6.30505884860508,-4.33522902210081));
#8626=CARTESIAN_POINT('Ctrl Pts',(0.541929400127819,6.24776718193879,-4.45821687574607));
#8627=CARTESIAN_POINT('Ctrl Pts',(-0.627008631335778,6.1331838486057,-4.47181195980492));
#8628=CARTESIAN_POINT('Ctrl Pts',(-1.21511855084784,6.07589218193929,-4.3623750618956));
#8629=CARTESIAN_POINT('Ctrl Pts',(-2.30925199488436,5.9613088486052,-3.92388536328634));
#8630=CARTESIAN_POINT('Ctrl Pts',(-2.81483021022013,5.90401718193932,-3.59496925151373));
#8631=CARTESIAN_POINT('Ctrl Pts',(-3.66474252897955,5.78943384860516,-2.76428328503534));
#8632=CARTESIAN_POINT('Ctrl Pts',(-4.0087148266721,5.73214218193892,-2.26281282911923));
#8633=CARTESIAN_POINT('Ctrl Pts',(-4.47975836595802,5.61755884860556,-1.1611387948422));
#8634=CARTESIAN_POINT('Ctrl Pts',(-4.60660845513052,5.56026718193889,-0.561353812600464));
#8635=CARTESIAN_POINT('Ctrl Pts',(-4.62020353922087,5.44568384860559,0.646433043808482));
#8636=CARTESIAN_POINT('Ctrl Pts',(-4.50690440572112,5.38839218193887,1.25395973267003));
#8637=CARTESIAN_POINT('Ctrl Pts',(-4.05354790547054,5.27380884860562,2.38398481094011));
#8638=CARTESIAN_POINT('Ctrl Pts',(-3.71363307734148,5.21651718193883,2.90602376850005));
#8639=CARTESIAN_POINT('Ctrl Pts',(-2.85547684333729,5.10193384860566,3.78340635482939));
#8640=CARTESIAN_POINT('Ctrl Pts',(-2.33754564515818,5.04464218193881,4.13837736882935));
#8641=CARTESIAN_POINT('Ctrl Pts',(-1.1999799766811,4.93005884860567,4.62428770981052));
#8642=CARTESIAN_POINT('Ctrl Pts',(-0.580778225062417,4.87276718193882,4.75500003451575));
#8643=CARTESIAN_POINT('Ctrl Pts',(0.665857456270481,4.75818384860567,4.76859511863605));
#8644=CARTESIAN_POINT('Ctrl Pts',(1.2928009144995,4.70089218193903,4.65143374954513));
#8645=CARTESIAN_POINT('Ctrl Pts',(2.45871762698856,4.58630884860546,4.18321044765625));
#8646=CARTESIAN_POINT('Ctrl Pts',(2.99721732678471,4.529017181939,3.83229690316695));
#8647=CARTESIAN_POINT('Ctrl Pts',(3.9020701806745,4.41443384860549,2.94667040164152));
#8648=CARTESIAN_POINT('Ctrl Pts',(4.2680399109909,4.35714218193895,2.41227846119283));
#8649=CARTESIAN_POINT('Ctrl Pts',(4.76881705365873,4.24255884860554,1.2388211585243));
#8650=CARTESIAN_POINT('Ctrl Pts',(4.90339161390277,4.18526718193866,0.600202637513305));
#8651=CARTESIAN_POINT('Ctrl Pts',(4.91698669804943,4.07068384860583,-0.685281868721417));
#8652=CARTESIAN_POINT('Ctrl Pts',(4.79596309336461,4.01339218193886,-1.33164209634213));
#8653=CARTESIAN_POINT('Ctrl Pts',(4.31287298984649,3.89880884860562,-2.53345044302389));
#8654=CARTESIAN_POINT('Ctrl Pts',(3.95096072898711,3.84151718193895,-3.08841088507667));
#8655=CARTESIAN_POINT('Ctrl Pts',(3.03786395995105,3.72693384860553,-4.02073400651229));
#8656=CARTESIAN_POINT('Ctrl Pts',(2.48701127721779,3.66964218193904,-4.39770245315732));
#8657=CARTESIAN_POINT('Ctrl Pts',(1.27766234037718,3.55505884860545,-4.91334639750207));
#8658=CARTESIAN_POINT('Ctrl Pts',(0.619627049962736,3.4977671819386,-5.05178319329073));
#8659=CARTESIAN_POINT('Ctrl Pts',(-0.704706281170879,3.38318384860588,-5.06537827746187));
#8660=CARTESIAN_POINT('Ctrl Pts',(-1.37048327818541,3.32589218193878,-4.94049243718524));
#8661=CARTESIAN_POINT('Ctrl Pts',(-2.60818325905853,3.21130884860571,-4.44253553203559));
#8662=CARTESIAN_POINT('Ctrl Pts',(-3.17960444337468,3.15401718193919,-4.06962455480154));
#8663=CARTESIAN_POINT('Ctrl Pts',(-4.13939783234407,3.03943384860528,-3.1290575182663));
#8664=CARTESIAN_POINT('Ctrl Pts',(-4.52736499532796,2.98214218193882,-2.5617440932366));
#8665=CARTESIAN_POINT('Ctrl Pts',(-5.05787574134119,2.86755884860567,-1.31650352223623));
#8666=CARTESIAN_POINT('Ctrl Pts',(-5.20017477267972,2.81026718193854,-0.639051462402516));
#8667=CARTESIAN_POINT('Ctrl Pts',(-5.21376985687329,2.69568384860595,0.724130693610728));
#8668=CARTESIAN_POINT('Ctrl Pts',(-5.08502178100269,2.638392181939,1.40932446003936));
#8669=CARTESIAN_POINT('Ctrl Pts',(-4.57219807422785,2.52380884860549,2.68291607508254));
#8670=CARTESIAN_POINT('Ctrl Pts',(-4.18828838061282,2.46651718193888,3.27079800167798));
#8671=CARTESIAN_POINT('Ctrl Pts',(-3.22025107658473,2.3519338486056,4.25806165817053));
#8672=CARTESIAN_POINT('Ctrl Pts',(-2.63647690924959,2.29464218193882,4.65702753750094));
#8673=CARTESIAN_POINT('Ctrl Pts',(-1.35534470410106,2.18005884860566,5.20240508517798));
#8674=CARTESIAN_POINT('Ctrl Pts',(-0.658475874835927,2.12276718193851,5.34856635206931));
#8675=CARTESIAN_POINT('Ctrl Pts',(0.743555106044213,2.00818384860598,5.3621614362841));
#8676=CARTESIAN_POINT('Ctrl Pts',(1.44816564189249,1.95089218193886,5.22955112482197));
#8677=CARTESIAN_POINT('Ctrl Pts',(2.75764889110733,1.83630884860562,4.70186061641829));
#8678=CARTESIAN_POINT('Ctrl Pts',(3.36199155998716,1.77901718193906,4.30695220641913));
#8679=CARTESIAN_POINT('Ctrl Pts',(4.37672548399112,1.66443384860542,3.3114446349081));
#8680=CARTESIAN_POINT('Ctrl Pts',(4.78669007967579,1.60714218193865,2.71120972526174));
#8681=CARTESIAN_POINT('Ctrl Pts',(5.3469344290129,1.49255884860583,1.39418588596674));
#8682=CARTESIAN_POINT('Ctrl Pts',(5.49695793145999,1.43526718193912,0.677900287260056));
#8683=CARTESIAN_POINT('Ctrl Pts',(5.51055301569383,1.32068384860537,-0.76297951846838));
#8684=CARTESIAN_POINT('Ctrl Pts',(5.37408046863567,1.26339218193915,-1.4870068237579));
#8685=CARTESIAN_POINT('Ctrl Pts',(4.83152315861431,1.14880884860534,-2.83238170711989));
#8686=CARTESIAN_POINT('Ctrl Pts',(4.42561603222875,1.09151718193863,-3.45318511829405));
#8687=CARTESIAN_POINT('Ctrl Pts',(3.40263819322818,0.976933848605856,-4.49538930981399));
#8688=CARTESIAN_POINT('Ctrl Pts',(2.78594254126256,0.919642181938648,-4.91635262185619));
#8689=CARTESIAN_POINT('Ctrl Pts',(1.43302706784377,0.805058848605838,-5.49146377284226));
#8690=CARTESIAN_POINT('Ctrl Pts',(0.697324699683797,0.747767181938915,-5.64534951085169));
#8691=CARTESIAN_POINT('Ctrl Pts',(-0.782403930892199,0.633183848605571,
-5.65894459510253));
#8692=CARTESIAN_POINT('Ctrl Pts',(-1.5258480056327,0.575892181939075,-5.51860981244762));
#8693=CARTESIAN_POINT('Ctrl Pts',(-2.90711452312302,0.46130884860541,-4.96118570081208));
#8694=CARTESIAN_POINT('Ctrl Pts',(-3.54437866826175,0.404017181938794,-4.5442798657039));
#8695=CARTESIAN_POINT('Ctrl Pts',(-4.07921590611891,0.346725515272242,-4.0190558047933));
#8696=CARTESIAN_POINT('Ctrl Pts',(-2.15943324690355,11.346909399206,-2.08633937475486));
#8697=CARTESIAN_POINT('Ctrl Pts',(-2.44157795049855,11.2895564378939,-1.81212632695763));
#8698=CARTESIAN_POINT('Ctrl Pts',(-2.67079732462106,11.2322034765833,-1.48005921159716));
#8699=CARTESIAN_POINT('Ctrl Pts',(-2.98550788648136,11.1175588486058,-0.748702056168519));
#8700=CARTESIAN_POINT('Ctrl Pts',(-3.07099283278885,11.0602671819391,-0.349756983242139));
#8701=CARTESIAN_POINT('Ctrl Pts',(-3.0818633980033,10.9456838486053,0.455650002839366));
#8702=CARTESIAN_POINT('Ctrl Pts',(-3.00720596150024,10.8883921819389,0.861795055291616));
#8703=CARTESIAN_POINT('Ctrl Pts',(-2.70531644391264,10.7738088486056,1.61902697886803));
#8704=CARTESIAN_POINT('Ctrl Pts',(-2.47816730458498,10.7165171819386,1.96980110153648));
#8705=CARTESIAN_POINT('Ctrl Pts',(-1.90261007970139,10.6019338486059,2.56073162722495));
#8706=CARTESIAN_POINT('Ctrl Pts',(-1.55440100825198,10.5446421819387,2.80062812645173));
#8707=CARTESIAN_POINT('Ctrl Pts',(-0.787543237963199,10.4300588486058,3.13003723037197));
#8708=CARTESIAN_POINT('Ctrl Pts',(-0.369181395757753,10.3727671819388,3.21938441215601));
#8709=CARTESIAN_POINT('Ctrl Pts',(0.475074415355009,10.2581838486057,3.23025497743655));
#8710=CARTESIAN_POINT('Ctrl Pts',(0.900636237067393,10.2008921819389,3.15173530532716));
#8711=CARTESIAN_POINT('Ctrl Pts',(1.69375979497017,10.0863088486056,2.83497898609545));
#8712=CARTESIAN_POINT('Ctrl Pts',(2.0609946597737,10.029017181939,2.59683113043342));
#8713=CARTESIAN_POINT('Ctrl Pts',(2.67939545311748,9.91443384860552,1.99380363798266));
#8714=CARTESIAN_POINT('Ctrl Pts',(2.93029066857928,9.8571421819389,1.62913382432459));
#8715=CARTESIAN_POINT('Ctrl Pts',(3.27456657425417,9.74255884860558,0.826384419768452));
#8716=CARTESIAN_POINT('Ctrl Pts',(3.36777599152708,9.68526718193864,0.388605808260406));
#8717=CARTESIAN_POINT('Ctrl Pts',(3.37864655686589,9.57068384860585,-0.49449882785769));
#8718=CARTESIAN_POINT('Ctrl Pts',(3.29626464915295,9.51339218193913,-0.939477418855915));
#8719=CARTESIAN_POINT('Ctrl Pts',(2.96464152827939,9.39880884860535,-1.76849261105957));
#8720=CARTESIAN_POINT('Ctrl Pts',(2.71549495627589,9.34151718193865,-2.15218821802195));
#8721=CARTESIAN_POINT('Ctrl Pts',(2.0849971962699,9.22693384860584,-2.79805927899898));
#8722=CARTESIAN_POINT('Ctrl Pts',(1.70386664038741,9.1696421819387,-3.05995321071421));
#8723=CARTESIAN_POINT('Ctrl Pts',(0.865225601583496,9.05505884860578,-3.419095918129));
#8724=CARTESIAN_POINT('Ctrl Pts',(0.408030220752219,8.99776718193874,-3.51616757090102));
#8725=CARTESIAN_POINT('Ctrl Pts',(-0.513923240349536,8.88318384860575,-3.52703813629236));
#8726=CARTESIAN_POINT('Ctrl Pts',(-0.978318600655415,8.82589218193907,-3.44079399297743));
#8727=CARTESIAN_POINT('Ctrl Pts',(-1.84322542713799,8.71130884860541,-3.09430407046464));
#8728=CARTESIAN_POINT('Ctrl Pts',(-2.24338177627906,8.65401718193906,-2.8341587821133));
#8729=CARTESIAN_POINT('Ctrl Pts',(-2.91672310487163,8.53943384860543,-2.1761907545622));
#8730=CARTESIAN_POINT('Ctrl Pts',(-3.18961575285625,8.4821421819388,-1.77859945644224));
#8731=CARTESIAN_POINT('Ctrl Pts',(-3.56362526199671,8.36755884860569,-0.904066783406526));
#8732=CARTESIAN_POINT('Ctrl Pts',(-3.66455915027763,8.3102671819386,-0.427454633233268));
#8733=CARTESIAN_POINT('Ctrl Pts',(-3.67542971571615,8.19568384860588,0.533347652830617));
#8734=CARTESIAN_POINT('Ctrl Pts',(-3.58532333680026,8.13839218193865,1.01715978246527));
#8735=CARTESIAN_POINT('Ctrl Pts',(-3.22396661265153,8.02380884860583,1.91795824320607));
#8736=CARTESIAN_POINT('Ctrl Pts',(-2.95282260794454,7.96651718193906,2.33457533454633));
#8737=CARTESIAN_POINT('Ctrl Pts',(-2.26738431286067,7.85193384860543,3.03538693073411));
#8738=CARTESIAN_POINT('Ctrl Pts',(-1.85333227248862,7.79464218193892,3.31927829500387));
#8739=CARTESIAN_POINT('Ctrl Pts',(-0.942907965238003,7.68005884860556,3.70815460585884));
#8740=CARTESIAN_POINT('Ctrl Pts',(-0.446879045704217,7.62276718193853,3.81295072965703));
#8741=CARTESIAN_POINT('Ctrl Pts',(0.552772065301601,7.50818384860596,3.82382129513715));
#8742=CARTESIAN_POINT('Ctrl Pts',(1.05600096428514,7.45089218193902,3.7298526806217));
#8743=CARTESIAN_POINT('Ctrl Pts',(1.99269105926411,7.33630884860546,3.35362915483982));
#8744=CARTESIAN_POINT('Ctrl Pts',(2.42576889282071,7.27901718193947,3.07148643377194));
#8745=CARTESIAN_POINT('Ctrl Pts',(3.15405075658949,7.16443384860501,2.35857787116297));
#8746=CARTESIAN_POINT('Ctrl Pts',(3.4489408371573,7.10714218193936,1.92806508852736));
#8747=CARTESIAN_POINT('Ctrl Pts',(3.85268394971518,6.99255884860513,0.981749147077123));
#8748=CARTESIAN_POINT('Ctrl Pts',(3.96134230903857,6.93526718193912,0.466303458167944));
#8749=CARTESIAN_POINT('Ctrl Pts',(3.97221287455602,6.82068384860537,-0.572196477765365));
#8750=CARTESIAN_POINT('Ctrl Pts',(3.87438202444231,6.76339218193869,-1.09484214611198));
#8751=CARTESIAN_POINT('Ctrl Pts',(3.48329169702894,6.6488088486058,-2.06742387531521));
#8752=CARTESIAN_POINT('Ctrl Pts',(3.19015025959274,6.5915171819388,-2.51696245110363));
#8753=CARTESIAN_POINT('Ctrl Pts',(2.44977142947187,6.47693384860569,-3.27271458243633));
#8754=CARTESIAN_POINT('Ctrl Pts',(2.00279790455941,6.41964218193941,-3.57860337931556));
#8755=CARTESIAN_POINT('Ctrl Pts',(1.02059032892293,6.30505884860508,-3.99721329356667));
#8756=CARTESIAN_POINT('Ctrl Pts',(0.485727870620802,6.24776718193879,-4.10973388842147));
#8757=CARTESIAN_POINT('Ctrl Pts',(-0.591620890218261,6.1331838486057,-4.12060445397352));
#8758=CARTESIAN_POINT('Ctrl Pts',(-1.13368332795069,6.07589218193929,-4.01891136825983));
#8759=CARTESIAN_POINT('Ctrl Pts',(-2.14215669135443,5.9613088486052,-3.61295423922114));
#8760=CARTESIAN_POINT('Ctrl Pts',(-2.60815600939102,5.90401718193932,-3.30881408541235));
#8761=CARTESIAN_POINT('Ctrl Pts',(-3.39137840827869,5.78943384860516,-2.54096498778195));
#8762=CARTESIAN_POINT('Ctrl Pts',(-3.70826592147772,5.73214218193892,-2.07753072058528));
#8763=CARTESIAN_POINT('Ctrl Pts',(-4.14174263741426,5.61755884860556,-1.05943151077492));
#8764=CARTESIAN_POINT('Ctrl Pts',(-4.25812546780629,5.56026718193889,-0.505152283069884));
#8765=CARTESIAN_POINT('Ctrl Pts',(-4.26899603338911,5.44568384860559,0.611045302667398));
#8766=CARTESIAN_POINT('Ctrl Pts',(-4.16344071207717,5.38839218193887,1.17252450979444));
#8767=CARTESIAN_POINT('Ctrl Pts',(-3.74261678141353,5.27380884860562,2.21688950738861));
#8768=CARTESIAN_POINT('Ctrl Pts',(-3.4274779112251,5.21651718193883,2.69934956768717));
#8769=CARTESIAN_POINT('Ctrl Pts',(-2.63215854609891,5.10193384860566,3.5100422341123));
#8770=CARTESIAN_POINT('Ctrl Pts',(-2.15226353660435,5.04464218193881,3.83792846364419));
#8771=CARTESIAN_POINT('Ctrl Pts',(-1.0982726926337,4.93005884860567,4.28627198125755));
#8772=CARTESIAN_POINT('Ctrl Pts',(-0.524576695510519,4.87276718193882,4.40651704719262));
#8773=CARTESIAN_POINT('Ctrl Pts',(0.630469715108076,4.75818384860567,4.41738761280318));
#8774=CARTESIAN_POINT('Ctrl Pts',(1.21136569164331,4.70089218193903,4.30797005589403));
#8775=CARTESIAN_POINT('Ctrl Pts',(2.29162232341768,4.58630884860546,3.87227932360639));
#8776=CARTESIAN_POINT('Ctrl Pts',(2.79054312598678,4.529017181939,3.5461417370364));
#8777=CARTESIAN_POINT('Ctrl Pts',(3.62870605994246,4.41443384860549,2.72335210441731));
#8778=CARTESIAN_POINT('Ctrl Pts',(3.96759100581396,4.35714218193895,2.22699635262072));
#8779=CARTESIAN_POINT('Ctrl Pts',(4.43080132509753,4.24255884860554,1.13711387449518));
#8780=CARTESIAN_POINT('Ctrl Pts',(4.55490862657983,4.18526718193866,0.544001107941954));
#8781=CARTESIAN_POINT('Ctrl Pts',(4.56577919221637,4.07068384860583,-0.649894127539557));
#8782=CARTESIAN_POINT('Ctrl Pts',(4.45249939970698,4.01339218193886,-1.25020687350361));
#8783=CARTESIAN_POINT('Ctrl Pts',(4.00194186580315,3.89880884860562,-2.36635513943533));
#8784=CARTESIAN_POINT('Ctrl Pts',(3.66480556284339,3.84151718193895,-2.88173668429245));
#8785=CARTESIAN_POINT('Ctrl Pts',(2.81454566274002,3.72693384860553,-3.74736988576655));
#8786=CARTESIAN_POINT('Ctrl Pts',(2.30172916862896,3.66964218193904,-4.09725354798759));
#8787=CARTESIAN_POINT('Ctrl Pts',(1.17595505636478,3.55505884860545,-4.57533066893367));
#8788=CARTESIAN_POINT('Ctrl Pts',(0.563425520373289,3.4977671819386,-4.70330020596852));
#8789=CARTESIAN_POINT('Ctrl Pts',(-0.669318539970923,3.38318384860588,-4.71417077162809));
#8790=CARTESIAN_POINT('Ctrl Pts',(-1.28904805536363,3.32589218193878,-4.59702874352091));
#8791=CARTESIAN_POINT('Ctrl Pts',(-2.44108795545323,3.21130884860571,-4.13160440799895));
#8792=CARTESIAN_POINT('Ctrl Pts',(-2.97293024260301,3.15401718193919,-3.78346938864651));
#8793=CARTESIAN_POINT('Ctrl Pts',(-3.86603371158577,3.03943384860528,-2.90573922106659));
#8794=CARTESIAN_POINT('Ctrl Pts',(-4.22691609016478,2.98214218193882,-2.37646198463267));
#8795=CARTESIAN_POINT('Ctrl Pts',(-4.71986001276623,2.86755884860567,-1.21479623823893));
#8796=CARTESIAN_POINT('Ctrl Pts',(-4.85169178535771,2.81026718193854,-0.582849932796644));
#8797=CARTESIAN_POINT('Ctrl Pts',(-4.86256235103931,2.69568384860595,0.688742952394343));
#8798=CARTESIAN_POINT('Ctrl Pts',(-4.74155808733321,2.638392181939,1.32788923723221));
#8799=CARTESIAN_POINT('Ctrl Pts',(-4.26126695019637,2.52380884860549,2.5158207714626));
#8800=CARTESIAN_POINT('Ctrl Pts',(-3.90213321444713,2.46651718193888,3.06412380091759));
#8801=CARTESIAN_POINT('Ctrl Pts',(-2.99693277939567,2.3519338486056,3.98469753740094));
#8802=CARTESIAN_POINT('Ctrl Pts',(-2.45119480063163,2.29464218193882,4.35657863234452));
#8803=CARTESIAN_POINT('Ctrl Pts',(-1.2536374201178,2.18005884860566,4.86438935659626));
#8804=CARTESIAN_POINT('Ctrl Pts',(-0.602274345215141,2.12276718193851,5.00008336474837));
#8805=CARTESIAN_POINT('Ctrl Pts',(0.708167364812911,2.00818384860598,5.01095393044905));
#8806=CARTESIAN_POINT('Ctrl Pts',(1.36673041909958,1.95089218193886,4.8860874311467));
#8807=CARTESIAN_POINT('Ctrl Pts',(2.59055358747315,1.83630884860562,4.39092949239261));
#8808=CARTESIAN_POINT('Ctrl Pts',(3.15531735923718,1.77901718193906,4.02079704024371));
#8809=CARTESIAN_POINT('Ctrl Pts',(4.10336136321113,1.66443384860542,3.08812633772876));
#8810=CARTESIAN_POINT('Ctrl Pts',(4.48624117452488,1.60714218193865,2.52592761663043));
#8811=CARTESIAN_POINT('Ctrl Pts',(5.00891870042567,1.49255884860583,1.29247860199682));
#8812=CARTESIAN_POINT('Ctrl Pts',(5.14847494413939,1.43526718193912,0.621698757625503));
#8813=CARTESIAN_POINT('Ctrl Pts',(5.15934550985844,1.32068384860537,-0.727591777223308));
#8814=CARTESIAN_POINT('Ctrl Pts',(5.0306167749558,1.26339218193915,-1.40557160097741));
#8815=CARTESIAN_POINT('Ctrl Pts',(4.52059203459322,1.14880884860534,-2.66528640347329));
#8816=CARTESIAN_POINT('Ctrl Pts',(4.13946086604337,1.09151718193863,-3.24651091755445));
#8817=CARTESIAN_POINT('Ctrl Pts',(3.17931989605881,0.976933848605856,-4.22202518902362));
#8818=CARTESIAN_POINT('Ctrl Pts',(2.60066043261983,0.919642181938648,-4.61590371671046));
#8819=CARTESIAN_POINT('Ctrl Pts',(1.33131978388528,0.805058848605838,-5.15344804424985));
#8820=CARTESIAN_POINT('Ctrl Pts',(0.641123170036348,0.747767181938915,-5.29686652353057));
#8821=CARTESIAN_POINT('Ctrl Pts',(-0.747016189634228,0.633183848605571,
-5.30773708926766));
#8822=CARTESIAN_POINT('Ctrl Pts',(-1.44441278286383,0.575892181939075,-5.17514611876316));
#8823=CARTESIAN_POINT('Ctrl Pts',(-2.74001921946479,0.46130884860541,-4.65025457679559));
#8824=CARTESIAN_POINT('Ctrl Pts',(-3.33770446803392,0.404017181938794,-4.25812469903555));
#8825=CARTESIAN_POINT('Ctrl Pts',(-3.83919674535392,0.346725515272242,-3.76431907311593));
#8826=CARTESIAN_POINT('Ctrl Pts',(-2.124655798183,11.0001838839337,-2.1190799629381));
#8827=CARTESIAN_POINT('Ctrl Pts',(-2.41109079938317,10.9428309226217,-1.84942416983751));
#8828=CARTESIAN_POINT('Ctrl Pts',(-2.64550594263638,10.885477961311,-1.52105845806273));
#8829=CARTESIAN_POINT('Ctrl Pts',(-2.97162798586693,10.7708333333336,-0.794830755283512));
#8830=CARTESIAN_POINT('Ctrl Pts',(-3.06332306119362,10.7135416666669,-0.397314139662748));
#8831=CARTESIAN_POINT('Ctrl Pts',(-3.08669273082211,10.5989583333331,0.407721033857582));
#8832=CARTESIAN_POINT('Ctrl Pts',(-3.01831935235521,10.5416666666666,0.814922877330024));
#8833=CARTESIAN_POINT('Ctrl Pts',(-2.728119788021,10.4270833333334,1.57659449107116));
#8834=CARTESIAN_POINT('Ctrl Pts',(-2.50637194487625,10.3697916666664,1.93074976622997));
#8835=CARTESIAN_POINT('Ctrl Pts',(-1.93991583267103,10.2552083333337,2.53025558222984));
#8836=CARTESIAN_POINT('Ctrl Pts',(-1.59540299717169,10.1979166666664,2.77534284559852));
#8837=CARTESIAN_POINT('Ctrl Pts',(-0.833671937081177,10.0833333333336,3.11615732976406));
#8838=CARTESIAN_POINT('Ctrl Pts',(-0.416738552178117,10.0260416666666,3.21171464055396));
#8839=CARTESIAN_POINT('Ctrl Pts',(0.427145446372979,9.91145833333345,3.23508431026218));
#8840=CARTESIAN_POINT('Ctrl Pts',(0.853764059103477,9.85416666666669,3.16284869617602));
#8841=CARTESIAN_POINT('Ctrl Pts',(1.65132730717562,9.73958333333332,2.85778233020993));
#8842=CARTESIAN_POINT('Ctrl Pts',(2.02194332446279,9.68229166666673,2.62503577071995));
#8843=CARTESIAN_POINT('Ctrl Pts',(2.64891940812677,9.56770833333328,2.03110939095704));
#8844=CARTESIAN_POINT('Ctrl Pts',(2.9050053877204,9.51041666666666,1.67013581324179));
#8845=CARTESIAN_POINT('Ctrl Pts',(3.26068667365192,9.39583333333334,0.872513118888943));
#8846=CARTESIAN_POINT('Ctrl Pts',(3.36010621991895,9.3385416666664,0.436162964680591));
#8847=CARTESIAN_POINT('Ctrl Pts',(3.38347588969759,9.22395833333361,-0.446569858875482));
#8848=CARTESIAN_POINT('Ctrl Pts',(3.30737803999626,9.16666666666689,-0.892605240889856));
#8849=CARTESIAN_POINT('Ctrl Pts',(2.98744487239941,9.05208333333312,-1.72606012326716));
#8850=CARTESIAN_POINT('Ctrl Pts',(2.74369959655829,8.99479166666641,-2.11313688270712));
#8851=CARTESIAN_POINT('Ctrl Pts',(2.1223029492484,8.8802083333336,-2.76758323401219));
#8852=CARTESIAN_POINT('Ctrl Pts',(1.74486862930228,8.82291666666647,-3.03466792985017));
#8853=CARTESIAN_POINT('Ctrl Pts',(0.911354300706321,8.70833333333354,-3.40521601753191));
#8854=CARTESIAN_POINT('Ctrl Pts',(0.455587377172263,8.6510416666665,-3.5084977992874));
#8855=CARTESIAN_POINT('Ctrl Pts',(-0.465994271367186,8.53645833333351,-3.53186746912954));
#8856=CARTESIAN_POINT('Ctrl Pts',(-0.93144642268745,8.47916666666683,-3.45190738381581));
#8857=CARTESIAN_POINT('Ctrl Pts',(-1.80079293934749,8.36458333333318,-3.11710741458959));
#8858=CARTESIAN_POINT('Ctrl Pts',(-2.20433044096071,8.30729166666683,-2.86236342239196));
#8859=CARTESIAN_POINT('Ctrl Pts',(-2.88624705988836,8.1927083333332,-2.21349650754444));
#8860=CARTESIAN_POINT('Ctrl Pts',(-3.1643304719878,8.13541666666656,-1.81960144535507));
#8861=CARTESIAN_POINT('Ctrl Pts',(-3.54974536140404,8.02083333333345,-0.950195482531384));
#8862=CARTESIAN_POINT('Ctrl Pts',(-3.65688937865929,7.96354166666637,-0.475011789653154));
#8863=CARTESIAN_POINT('Ctrl Pts',(-3.68025904855805,7.84895833333365,0.485418683848109));
#8864=CARTESIAN_POINT('Ctrl Pts',(-3.59643672763413,7.79166666666665,0.970287604495667));
#8865=CARTESIAN_POINT('Ctrl Pts',(-3.246769956781,7.67708333333337,1.8755257554172));
#8866=CARTESIAN_POINT('Ctrl Pts',(-2.98102724821984,7.61979166666659,2.29552399922486));
#8867=CARTESIAN_POINT('Ctrl Pts',(-2.30469006584627,7.50520833333343,3.00491088575395));
#8868=CARTESIAN_POINT('Ctrl Pts',(-1.89433426139971,7.44791666666668,3.29399301413121));
#8869=CARTESIAN_POINT('Ctrl Pts',(-0.989036664364609,7.33333333333333,3.69427470527038));
#8870=CARTESIAN_POINT('Ctrl Pts',(-0.49443620212397,7.27604166666629,3.80528095803426));
#8871=CARTESIAN_POINT('Ctrl Pts',(0.50484309631896,7.16145833333372,3.82865062798349));
#8872=CARTESIAN_POINT('Ctrl Pts',(1.00912878631411,7.10416666666678,3.74096607145172));
#8873=CARTESIAN_POINT('Ctrl Pts',(1.95025857147667,6.98958333333323,3.37643249897315));
#8874=CARTESIAN_POINT('Ctrl Pts',(2.38671755749636,6.93229166666724,3.09969107404422));
#8875=CARTESIAN_POINT('Ctrl Pts',(3.12357471161222,6.81770833333277,2.39588362415159));
#8876=CARTESIAN_POINT('Ctrl Pts',(3.42365555628099,6.76041666666712,1.96906707743673));
#8877=CARTESIAN_POINT('Ctrl Pts',(3.83880404913035,6.64583333333289,1.02787784620545));
#8878=CARTESIAN_POINT('Ctrl Pts',(3.95367253741186,6.58854166666688,0.51386061458762));
#8879=CARTESIAN_POINT('Ctrl Pts',(3.97704220740629,6.47395833333313,-0.524267508782646));
#8880=CARTESIAN_POINT('Ctrl Pts',(3.88549541526866,6.41666666666645,-1.04796996813959));
#8881=CARTESIAN_POINT('Ctrl Pts',(3.50609504116593,6.30208333333356,-2.02499138752914));
#8882=CARTESIAN_POINT('Ctrl Pts',(3.2183548998624,6.24479166666656,-2.47791111577681));
#8883=CARTESIAN_POINT('Ctrl Pts',(2.48707718246311,6.13020833333345,-3.24223853746153));
#8884=CARTESIAN_POINT('Ctrl Pts',(2.04379989346725,6.07291666666717,-3.55331809843599));
#8885=CARTESIAN_POINT('Ctrl Pts',(1.06671902805278,5.95833333333284,-3.9833333929851));
#8886=CARTESIAN_POINT('Ctrl Pts',(0.533285027040294,5.90104166666655,-4.10206411679133));
#8887=CARTESIAN_POINT('Ctrl Pts',(-0.543691921235359,5.78645833333346,-4.12543378682723));
#8888=CARTESIAN_POINT('Ctrl Pts',(-1.08681114997705,5.72916666666705,-4.03002475908303));
#8889=CARTESIAN_POINT('Ctrl Pts',(-2.0997242035696,5.61458333333296,-3.63575758336128));
#8890=CARTESIAN_POINT('Ctrl Pts',(-2.56910467406188,5.55729166666709,-3.33701872567955));
#8891=CARTESIAN_POINT('Ctrl Pts',(-3.36090236330622,5.44270833333292,-2.57827074077566));
#8892=CARTESIAN_POINT('Ctrl Pts',(-3.68298064059524,5.38541666666669,-2.11853270949184));
#8893=CARTESIAN_POINT('Ctrl Pts',(-4.12786273683561,5.27083333333332,-1.10556020990605));
#8894=CARTESIAN_POINT('Ctrl Pts',(-4.25045569617289,5.21354166666665,-0.552709439489368));
#8895=CARTESIAN_POINT('Ctrl Pts',(-4.27382536624608,5.09895833333335,0.563116333684488));
#8896=CARTESIAN_POINT('Ctrl Pts',(-4.17455410289751,5.04166666666663,1.12565233181968));
#8897=CARTESIAN_POINT('Ctrl Pts',(-3.76542012555652,4.92708333333338,2.17445701960491));
#8898=CARTESIAN_POINT('Ctrl Pts',(-3.45568255149002,4.86979166666659,2.66029823235588));
#8899=CARTESIAN_POINT('Ctrl Pts',(-2.6694642990949,4.75520833333342,3.47956618914197));
#8900=CARTESIAN_POINT('Ctrl Pts',(-2.19326552550957,4.69791666666658,3.81264318275876));
#8901=CARTESIAN_POINT('Ctrl Pts',(-1.14440139176617,4.58333333333343,4.27239208068185));
#8902=CARTESIAN_POINT('Ctrl Pts',(-0.572133851929879,4.52604166666658,4.39884727555618));
#8903=CARTESIAN_POINT('Ctrl Pts',(0.582540746125043,4.41145833333343,4.42221694566319));
#8904=CARTESIAN_POINT('Ctrl Pts',(1.16449351366757,4.35416666666679,4.31908344671154));
#8905=CARTESIAN_POINT('Ctrl Pts',(2.24918983563495,4.23958333333322,3.89508266775222));
#8906=CARTESIAN_POINT('Ctrl Pts',(2.75149179065353,4.18229166666676,3.57434637729919));
#8907=CARTESIAN_POINT('Ctrl Pts',(3.59823001497408,4.06770833333325,2.76065785741543));
#8908=CARTESIAN_POINT('Ctrl Pts',(3.94230572492611,4.01041666666671,2.26799834152485));
#8909=CARTESIAN_POINT('Ctrl Pts',(4.41692142452426,3.8958333333333,1.18324257362874));
#8910=CARTESIAN_POINT('Ctrl Pts',(4.54723885494094,3.83854166666642,0.591558264361257));
#8911=CARTESIAN_POINT('Ctrl Pts',(4.57060852507883,3.72395833333359,-0.601965158556466));
#8912=CARTESIAN_POINT('Ctrl Pts',(4.46361279052205,3.66666666666662,-1.20333469552689));
#8913=CARTESIAN_POINT('Ctrl Pts',(4.02474520995143,3.55208333333339,-2.32392265165357));
#8914=CARTESIAN_POINT('Ctrl Pts',(3.69301020310442,3.49479166666671,-2.84268534895739));
#8915=CARTESIAN_POINT('Ctrl Pts',(2.85185141573989,3.38020833333329,-3.71689384079999));
#8916=CARTESIAN_POINT('Ctrl Pts',(2.34273115753217,3.3229166666668,-4.07196826709743));
#8917=CARTESIAN_POINT('Ctrl Pts',(1.22208375549926,3.20833333333321,-4.56145076836271));
#8918=CARTESIAN_POINT('Ctrl Pts',(0.610982676792531,3.15104166666636,-4.6956304343271));
#8919=CARTESIAN_POINT('Ctrl Pts',(-0.621389570987771,3.03645833333365,-4.71900010449308));
#8920=CARTESIAN_POINT('Ctrl Pts',(-1.24217587738614,2.97916666666654,-4.60814213433379));
#8921=CARTESIAN_POINT('Ctrl Pts',(-2.39865546767225,2.86458333333347,-4.15440775214941));
#8922=CARTESIAN_POINT('Ctrl Pts',(-2.93387890726637,2.80729166666695,-3.81167402890586));
#8923=CARTESIAN_POINT('Ctrl Pts',(-3.83555766662078,2.69270833333305,-2.94304497406814));
#8924=CARTESIAN_POINT('Ctrl Pts',(-4.20163080927273,2.63541666666658,-2.41746397353493));
#8925=CARTESIAN_POINT('Ctrl Pts',(-4.70598011219716,2.52083333333343,-1.26092493737436));
#8926=CARTESIAN_POINT('Ctrl Pts',(-4.84402201371418,2.4635416666663,-0.630407089215845));
#8927=CARTESIAN_POINT('Ctrl Pts',(-4.86739168390641,2.34895833333371,0.64081398341115));
#8928=CARTESIAN_POINT('Ctrl Pts',(-4.75267147814405,2.29166666666676,1.28101705925391));
#8929=CARTESIAN_POINT('Ctrl Pts',(-4.28407029434887,2.17708333333325,2.47338828368244));
#8930=CARTESIAN_POINT('Ctrl Pts',(-3.93033785470491,2.11979166666664,3.0250724655795));
#8931=CARTESIAN_POINT('Ctrl Pts',(-3.0342385323988,2.00520833333337,3.95422149243741));
#8932=CARTESIAN_POINT('Ctrl Pts',(-2.49219678953305,1.94791666666658,4.33129335145034));
#8933=CARTESIAN_POINT('Ctrl Pts',(-1.29976611925407,1.83333333333343,4.85050945602931));
#8934=CARTESIAN_POINT('Ctrl Pts',(-0.6498315016342,1.77604166666627,4.99241359310244));
#8935=CARTESIAN_POINT('Ctrl Pts',(0.660238395829575,1.66145833333374,5.01578326331855));
#8936=CARTESIAN_POINT('Ctrl Pts',(1.31985824112059,1.60416666666663,4.89720082195578));
#8937=CARTESIAN_POINT('Ctrl Pts',(2.54812109969368,1.48958333333338,4.41373283654687));
#8938=CARTESIAN_POINT('Ctrl Pts',(3.1162660238978,1.43229166666683,4.04900168050008));
#8939=CARTESIAN_POINT('Ctrl Pts',(4.07288531824889,1.31770833333318,3.1254320907333));
#8940=CARTESIAN_POINT('Ctrl Pts',(4.460955893629,1.26041666666641,2.56692960553103));
#8941=CARTESIAN_POINT('Ctrl Pts',(4.99503879986042,1.1458333333336,1.33860730113391));
#8942=CARTESIAN_POINT('Ctrl Pts',(5.14080517249185,1.08854166666688,0.669255914044516));
#8943=CARTESIAN_POINT('Ctrl Pts',(5.16417484272955,0.973958333333134,-0.679662808239928));
#8944=CARTESIAN_POINT('Ctrl Pts',(5.04173016576313,0.916666666666909,-1.35869942299763));
#8945=CARTESIAN_POINT('Ctrl Pts',(4.54339537874923,0.8020833333331,-2.62285391569459));
#8946=CARTESIAN_POINT('Ctrl Pts',(4.16766550629842,0.744791666666392,-3.20745958221381));
#8947=CARTESIAN_POINT('Ctrl Pts',(3.21662564906467,0.630208333333619,-4.19154914406263));
#8948=CARTESIAN_POINT('Ctrl Pts',(2.6416624215197,0.572916666666411,-4.59061843581319));
#8949=CARTESIAN_POINT('Ctrl Pts',(1.3774484830231,0.4583333333336,-5.13956814368599));
#8950=CARTESIAN_POINT('Ctrl Pts',(0.688680326455284,0.401041666666677,-5.28919675188146));
#8951=CARTESIAN_POINT('Ctrl Pts',(-0.69908722065077,0.286458333333334,-5.31256642214034));
#8952=CARTESIAN_POINT('Ctrl Pts',(-1.39754060488348,0.229166666666838,-5.1862595095691));
#8953=CARTESIAN_POINT('Ctrl Pts',(-2.69758673168668,0.114583333333173,-4.67305792095299));
#8954=CARTESIAN_POINT('Ctrl Pts',(-3.29865313262765,0.0572916666665569,
-4.28632933922004));
#8955=CARTESIAN_POINT('Ctrl Pts',(-3.80443305520312,5.20417042793042E-15,
-3.79707426974638));
#8956=CARTESIAN_POINT('Ctrl Pts',(-2.08987834946245,10.6534583686615,-2.15182055112134));
#8957=CARTESIAN_POINT('Ctrl Pts',(-2.38060364826779,10.5961054073494,-1.88672201271739));
#8958=CARTESIAN_POINT('Ctrl Pts',(-2.62021456065169,10.5387524460388,-1.5620577045283));
#8959=CARTESIAN_POINT('Ctrl Pts',(-2.9577480852525,10.4241078180613,-0.840959454398505));
#8960=CARTESIAN_POINT('Ctrl Pts',(-3.05565328959838,10.3668161513947,-0.444871296083357));
#8961=CARTESIAN_POINT('Ctrl Pts',(-3.09152206364091,10.2522328180609,0.359792064875797));
#8962=CARTESIAN_POINT('Ctrl Pts',(-3.02943274321019,10.1949411513944,0.768050699368431));
#8963=CARTESIAN_POINT('Ctrl Pts',(-2.75092313212936,10.0803578180611,1.53416200327429));
#8964=CARTESIAN_POINT('Ctrl Pts',(-2.53457658516751,10.0230661513941,1.89169843092347));
#8965=CARTESIAN_POINT('Ctrl Pts',(-1.97722158564067,9.90848281806141,2.49977953723472));
#8966=CARTESIAN_POINT('Ctrl Pts',(-1.6364049860914,9.8511911513942,2.75005756474531));
#8967=CARTESIAN_POINT('Ctrl Pts',(-0.879800636199156,9.73660781806133,3.10227742915614));
#8968=CARTESIAN_POINT('Ctrl Pts',(-0.46429570859848,9.67931615139432,3.2040448689519));
#8969=CARTESIAN_POINT('Ctrl Pts',(0.379216477390949,9.56473281806121,3.2399136430878));
#8970=CARTESIAN_POINT('Ctrl Pts',(0.806891881139562,9.50744115139445,3.17396208702488));
#8971=CARTESIAN_POINT('Ctrl Pts',(1.60889481938107,9.39285781806108,2.8805856743244));
#8972=CARTESIAN_POINT('Ctrl Pts',(1.98289198915187,9.33556615139449,2.65324041100648));
#8973=CARTESIAN_POINT('Ctrl Pts',(2.61844336313606,9.22098281806105,2.06841514393141));
#8974=CARTESIAN_POINT('Ctrl Pts',(2.87972010686153,9.16369115139443,1.71113780215899));
#8975=CARTESIAN_POINT('Ctrl Pts',(3.24680677304967,9.0491078180611,0.918641818009435));
#8976=CARTESIAN_POINT('Ctrl Pts',(3.35243644831083,8.99181615139416,0.483720121100777));
#8977=CARTESIAN_POINT('Ctrl Pts',(3.38830522252928,8.87723281806137,-0.398640889893273));
#8978=CARTESIAN_POINT('Ctrl Pts',(3.31849143083958,8.81994115139465,-0.845733062923796));
#8979=CARTESIAN_POINT('Ctrl Pts',(3.01024821651943,8.70535781806088,-1.68362763547476));
#8980=CARTESIAN_POINT('Ctrl Pts',(2.77190423684068,8.64806615139417,-2.0740855473923));
#8981=CARTESIAN_POINT('Ctrl Pts',(2.15960870222691,8.53348281806136,-2.73710718902539));
#8982=CARTESIAN_POINT('Ctrl Pts',(1.78587061821714,8.47619115139423,-3.00938264898613));
#8983=CARTESIAN_POINT('Ctrl Pts',(0.957482999829145,8.36160781806131,-3.39133611693482));
#8984=CARTESIAN_POINT('Ctrl Pts',(0.503144533592307,8.30431615139426,-3.50082802767378));
#8985=CARTESIAN_POINT('Ctrl Pts',(-0.418065302384836,8.18973281806127,-3.53669680196673));
#8986=CARTESIAN_POINT('Ctrl Pts',(-0.884574244719486,8.1324411513946,-3.4630207746542));
#8987=CARTESIAN_POINT('Ctrl Pts',(-1.75836045155699,8.01785781806094,-3.13991075871454));
#8988=CARTESIAN_POINT('Ctrl Pts',(-2.16527910564236,7.96056615139459,-2.89056806267063));
#8989=CARTESIAN_POINT('Ctrl Pts',(-2.85577101490508,7.84598281806096,-2.25080226052668));
#8990=CARTESIAN_POINT('Ctrl Pts',(-3.13904519111934,7.78869115139432,-1.8606034342679));
#8991=CARTESIAN_POINT('Ctrl Pts',(-3.53586546081137,7.67410781806122,-0.996324181656243));
#8992=CARTESIAN_POINT('Ctrl Pts',(-3.64921960704095,7.61681615139413,-0.52256894607304));
#8993=CARTESIAN_POINT('Ctrl Pts',(-3.68508838139996,7.50223281806141,0.437489714865601));
#8994=CARTESIAN_POINT('Ctrl Pts',(-3.60755011846799,7.44494115139464,0.923415426526065));
#8995=CARTESIAN_POINT('Ctrl Pts',(-3.26957330091048,7.33035781806089,1.83309326762834));
#8996=CARTESIAN_POINT('Ctrl Pts',(-3.00923188849514,7.27306615139411,2.25647266390339));
#8997=CARTESIAN_POINT('Ctrl Pts',(-2.34199581883187,7.15848281806142,2.9744348407738));
#8998=CARTESIAN_POINT('Ctrl Pts',(-1.93533625031079,7.10119115139444,3.26870773325855));
#8999=CARTESIAN_POINT('Ctrl Pts',(-1.03516536349122,6.98660781806109,3.68039480468192));
#9000=CARTESIAN_POINT('Ctrl Pts',(-0.541993358543724,6.92931615139405,3.79761118641148));
#9001=CARTESIAN_POINT('Ctrl Pts',(0.45691412733632,6.81473281806148,3.83347996082984));
#9002=CARTESIAN_POINT('Ctrl Pts',(0.962256608343087,6.75744115139454,3.75207946228173));
#9003=CARTESIAN_POINT('Ctrl Pts',(1.90782608368924,6.64285781806099,3.39923584310647));
#9004=CARTESIAN_POINT('Ctrl Pts',(2.34766622217201,6.585566151395,3.12789571431651));
#9005=CARTESIAN_POINT('Ctrl Pts',(3.09309866663495,6.47098281806054,2.4331893771402));
#9006=CARTESIAN_POINT('Ctrl Pts',(3.39837027540469,6.41369115139488,2.01006906634609));
#9007=CARTESIAN_POINT('Ctrl Pts',(3.82492414854553,6.29910781806065,1.07400654533378));
#9008=CARTESIAN_POINT('Ctrl Pts',(3.94600276578516,6.24181615139464,0.561417771007294));
#9009=CARTESIAN_POINT('Ctrl Pts',(3.98187154025657,6.1272328180609,-0.476338539799928));
#9010=CARTESIAN_POINT('Ctrl Pts',(3.89660880609501,6.06994115139421,-1.00109779016719));
#9011=CARTESIAN_POINT('Ctrl Pts',(3.52889838530292,5.95535781806132,-1.98255889974307));
#9012=CARTESIAN_POINT('Ctrl Pts',(3.24655954013207,5.89806615139432,-2.43885978044999));
#9013=CARTESIAN_POINT('Ctrl Pts',(2.52438293545435,5.78348281806122,-3.21176249248673));
#9014=CARTESIAN_POINT('Ctrl Pts',(2.08480188237509,5.72619115139493,-3.52803281755643));
#9015=CARTESIAN_POINT('Ctrl Pts',(1.11284772718263,5.6116078180606,-3.96945349240354));
#9016=CARTESIAN_POINT('Ctrl Pts',(0.580842183459787,5.55431615139431,-4.0943943451612));
#9017=CARTESIAN_POINT('Ctrl Pts',(-0.495762952252458,5.43973281806122,-4.13026311968094));
#9018=CARTESIAN_POINT('Ctrl Pts',(-1.03993897200342,5.38244115139481,-4.04113814990623));
#9019=CARTESIAN_POINT('Ctrl Pts',(-2.05729171578477,5.26785781806072,-3.65856092750142));
#9020=CARTESIAN_POINT('Ctrl Pts',(-2.53005333873273,5.21056615139485,-3.36522336594676));
#9021=CARTESIAN_POINT('Ctrl Pts',(-3.33042631833374,5.09598281806069,-2.61557649376936));
#9022=CARTESIAN_POINT('Ctrl Pts',(-3.65769535971276,5.03869115139445,-2.1595346983984));
#9023=CARTESIAN_POINT('Ctrl Pts',(-4.11398283625697,4.92410781806109,-1.15168890903718));
#9024=CARTESIAN_POINT('Ctrl Pts',(-4.24278592453948,4.86681615139442,-0.600266595908851));
#9025=CARTESIAN_POINT('Ctrl Pts',(-4.27865469910306,4.75223281806112,0.515187364701578));
#9026=CARTESIAN_POINT('Ctrl Pts',(-4.18566749371785,4.69494115139439,1.07878015384492));
#9027=CARTESIAN_POINT('Ctrl Pts',(-3.78822346969952,4.58035781806114,2.13202453182121));
#9028=CARTESIAN_POINT('Ctrl Pts',(-3.48388719175493,4.52306615139435,2.62124689702459));
#9029=CARTESIAN_POINT('Ctrl Pts',(-2.70677005209088,4.40848281806118,3.44909014417165));
#9030=CARTESIAN_POINT('Ctrl Pts',(-2.2342675144148,4.35119115139434,3.78735790187333));
#9031=CARTESIAN_POINT('Ctrl Pts',(-1.19053009089864,4.2366078180612,4.25851218010615));
#9032=CARTESIAN_POINT('Ctrl Pts',(-0.61969100834924,4.17931615139434,4.39117750391975));
#9033=CARTESIAN_POINT('Ctrl Pts',(0.53461177714201,4.06473281806119,4.42704627852319));
#9034=CARTESIAN_POINT('Ctrl Pts',(1.11762133569182,4.00744115139456,4.33019683752905));
#9035=CARTESIAN_POINT('Ctrl Pts',(2.20675734785223,3.89285781806098,3.91788601189805));
#9036=CARTESIAN_POINT('Ctrl Pts',(2.71244045532029,3.83556615139452,3.60255101756198));
#9037=CARTESIAN_POINT('Ctrl Pts',(3.56775397000571,3.72098281806102,2.79796361041354));
#9038=CARTESIAN_POINT('Ctrl Pts',(3.91702044403826,3.66369115139447,2.30900033042897));
#9039=CARTESIAN_POINT('Ctrl Pts',(4.40304152395098,3.54910781806106,1.22937127276231));
#9040=CARTESIAN_POINT('Ctrl Pts',(4.53956908330205,3.49181615139418,0.63911542078056));
#9041=CARTESIAN_POINT('Ctrl Pts',(4.5754378579413,3.37723281806136,-0.554036189573376));
#9042=CARTESIAN_POINT('Ctrl Pts',(4.47472618133712,3.31994115139439,-1.15646251755018));
#9043=CARTESIAN_POINT('Ctrl Pts',(4.0475485540997,3.20535781806115,-2.28149016387182));
#9044=CARTESIAN_POINT('Ctrl Pts',(3.72121484336545,3.14806615139448,-2.80363401362233));
#9045=CARTESIAN_POINT('Ctrl Pts',(2.88915716873977,3.03348281806106,-3.68641779583343));
#9046=CARTESIAN_POINT('Ctrl Pts',(2.38373314643537,2.97619115139456,-4.04668298620726));
#9047=CARTESIAN_POINT('Ctrl Pts',(1.26821245463375,2.86160781806097,-4.54757086779175));
#9048=CARTESIAN_POINT('Ctrl Pts',(0.658539833211772,2.80431615139412,-4.68796066268569));
#9049=CARTESIAN_POINT('Ctrl Pts',(-0.573460602004618,2.68973281806141,-4.72382943735807));
#9050=CARTESIAN_POINT('Ctrl Pts',(-1.19530369940865,2.6324411513943,-4.61925552514667));
#9051=CARTESIAN_POINT('Ctrl Pts',(-2.35622297989128,2.51785781806124,-4.17721109629987));
#9052=CARTESIAN_POINT('Ctrl Pts',(-2.89482757192974,2.46056615139471,-3.83987866916521));
#9053=CARTESIAN_POINT('Ctrl Pts',(-3.8050816216558,2.34598281806081,-2.98035072706969));
#9054=CARTESIAN_POINT('Ctrl Pts',(-4.17634552838067,2.28869115139434,-2.4584659624372));
#9055=CARTESIAN_POINT('Ctrl Pts',(-4.6921002116281,2.1741078180612,-1.30705363650978));
#9056=CARTESIAN_POINT('Ctrl Pts',(-4.83635224207065,2.11681615139406,-0.677964245635046));
#9057=CARTESIAN_POINT('Ctrl Pts',(-4.87222101677351,2.00223281806147,0.592885014427957));
#9058=CARTESIAN_POINT('Ctrl Pts',(-4.76378486895489,1.94494115139452,1.23414488127561));
#9059=CARTESIAN_POINT('Ctrl Pts',(-4.30687363850137,1.83035781806102,2.43095579590228));
#9060=CARTESIAN_POINT('Ctrl Pts',(-3.95854249496268,1.77306615139441,2.98602113024142));
#9061=CARTESIAN_POINT('Ctrl Pts',(-3.07154428540192,1.65848281806113,3.92374544747388));
#9062=CARTESIAN_POINT('Ctrl Pts',(-2.53319877843447,1.60119115139435,4.30600807055617));
#9063=CARTESIAN_POINT('Ctrl Pts',(-1.34589481839034,1.48660781806119,4.83662955546236));
#9064=CARTESIAN_POINT('Ctrl Pts',(-0.697388658053259,1.42931615139403,4.9847438214565));
#9065=CARTESIAN_POINT('Ctrl Pts',(0.61230942684624,1.3147328180615,5.02061259618806));
#9066=CARTESIAN_POINT('Ctrl Pts',(1.27298606314159,1.25744115139439,4.90831421276487));
#9067=CARTESIAN_POINT('Ctrl Pts',(2.50568861191421,1.14285781806115,4.43653618070112));
#9068=CARTESIAN_POINT('Ctrl Pts',(3.07721468855841,1.08556615139459,4.07720632075644));
#9069=CARTESIAN_POINT('Ctrl Pts',(4.04240927328666,0.970982818060947,3.16273784373784));
#9070=CARTESIAN_POINT('Ctrl Pts',(4.43567061273313,0.913691151394175,2.60793159443164));
#9071=CARTESIAN_POINT('Ctrl Pts',(4.98115889929517,0.79910781806136,1.384736000271));
#9072=CARTESIAN_POINT('Ctrl Pts',(5.13313540084431,0.741816151394642,0.716813070463529));
#9073=CARTESIAN_POINT('Ctrl Pts',(5.16900417560066,0.627232818060896,-0.631733839256547));
#9074=CARTESIAN_POINT('Ctrl Pts',(5.05284355657047,0.569941151394671,-1.31182724501786));
#9075=CARTESIAN_POINT('Ctrl Pts',(4.56619872290524,0.455357818060863,-2.5804214279159));
#9076=CARTESIAN_POINT('Ctrl Pts',(4.19587014655347,0.398066151394155,-3.16840824687318));
#9077=CARTESIAN_POINT('Ctrl Pts',(3.25393140207052,0.283482818061382,-4.16107309910165));
#9078=CARTESIAN_POINT('Ctrl Pts',(2.68266441041957,0.226191151394174,-4.56533315491593));
#9079=CARTESIAN_POINT('Ctrl Pts',(1.42357718216092,0.111607818061363,-5.12568824312213));
#9080=CARTESIAN_POINT('Ctrl Pts',(0.736237482874218,0.0543161513944401,
-5.28152698023234));
#9081=CARTESIAN_POINT('Ctrl Pts',(-0.651158251667311,-0.0602671819389035,
-5.31739575501303));
#9082=CARTESIAN_POINT('Ctrl Pts',(-1.35066842690312,-0.117558848605399,
-5.19737290037505));
#9083=CARTESIAN_POINT('Ctrl Pts',(-2.65515424390857,-0.232142181939065,
-4.69586126511038));
#9084=CARTESIAN_POINT('Ctrl Pts',(-3.25960179722137,-0.28943384860568,-4.31453397940454));
#9085=CARTESIAN_POINT('Ctrl Pts',(-3.76966936505231,-0.346725515272232,
-3.82982946637684));
#9086=CARTESIAN_POINT('Ctrl Pts',(-2.32979046439652,10.6534583686615,-2.40665810101083));
#9087=CARTESIAN_POINT('Ctrl Pts',(-2.65390980629198,10.5961054073494,-2.1101216920847));
#9088=CARTESIAN_POINT('Ctrl Pts',(-2.92064337015263,10.5387524460388,-1.74738451990478));
#9089=CARTESIAN_POINT('Ctrl Pts',(-3.29576381367816,10.4241078180613,-0.942666738728406));
#9090=CARTESIAN_POINT('Ctrl Pts',(-3.40413627693083,10.3668161513947,-0.501072825334149));
#9091=CARTESIAN_POINT('Ctrl Pts',(-3.44272956946446,10.2522328180609,0.39517980573707));
#9092=CARTESIAN_POINT('Ctrl Pts',(-3.37289643675743,10.1949411513944,0.849485922498689));
#9093=CARTESIAN_POINT('Ctrl Pts',(-3.06185425628309,10.0803578180611,1.70125730657109));
#9094=CARTESIAN_POINT('Ctrl Pts',(-2.82073175110235,10.0230661513941,2.0983726319291));
#9095=CARTESIAN_POINT('Ctrl Pts',(-2.2005398830606,9.90848281806141,2.77314365775904));
#9096=CARTESIAN_POINT('Ctrl Pts',(-1.82168709441022,9.8511911513942,3.05050647003645));
#9097=CARTESIAN_POINT('Ctrl Pts',(-0.98150792048159,9.73660781806133,3.44029315760313));
#9098=CARTESIAN_POINT('Ctrl Pts',(-0.520497237899657,9.67931615139432,3.55252785628273));
#9099=CARTESIAN_POINT('Ctrl Pts',(0.41460421830261,9.56473281806121,3.59112114891296));
#9100=CARTESIAN_POINT('Ctrl Pts',(0.888327104224163,9.50744115139445,3.51742578058933));
#9101=CARTESIAN_POINT('Ctrl Pts',(1.77599012272354,9.39285781806108,3.19151679846092));
#9102=CARTESIAN_POINT('Ctrl Pts',(2.18956619012306,9.33556615139449,2.93939557697384));
#9103=CARTESIAN_POINT('Ctrl Pts',(2.89180748369484,9.22098281806105,2.29173344131881));
#9104=CARTESIAN_POINT('Ctrl Pts',(3.18016901213384,9.16369115139443,1.8964199105197));
#9105=CARTESIAN_POINT('Ctrl Pts',(3.58482250151549,9.0491078180611,1.02034910224998));
#9106=CARTESIAN_POINT('Ctrl Pts',(3.70091943564033,8.99181615139416,0.539921650446381));
#9107=CARTESIAN_POINT('Ctrl Pts',(3.73951272835577,8.87723281806137,-0.434028630849363));
#9108=CARTESIAN_POINT('Ctrl Pts',(3.66195512441954,8.81994115139465,-0.927168285967855));
#9109=CARTESIAN_POINT('Ctrl Pts',(3.32117934064045,8.70535781806088,-1.85072293885776));
#9110=CARTESIAN_POINT('Ctrl Pts',(3.05805940283662,8.64806615139417,-2.28075974833291));
#9111=CARTESIAN_POINT('Ctrl Pts',(2.38292699958574,8.53348281806136,-3.01047130961474));
#9112=CARTESIAN_POINT('Ctrl Pts',(1.97115272661516,8.47619115139423,-3.30983155424184));
#9113=CARTESIAN_POINT('Ctrl Pts',(1.05919028403238,8.36160781806131,-3.72935184541724));
#9114=CARTESIAN_POINT('Ctrl Pts',(0.559346062977529,8.30431615139426,-3.8493110150021));
#9115=CARTESIAN_POINT('Ctrl Pts',(-0.453453043380547,8.18973281806127,-3.8879043077944));
#9116=CARTESIAN_POINT('Ctrl Pts',(-0.966009467727636,8.1324411513946,-3.80648446824784));
#9117=CARTESIAN_POINT('Ctrl Pts',(-1.92545575497591,8.01785781806094,-3.45084188282187));
#9118=CARTESIAN_POINT('Ctrl Pts',(-2.37195330655562,7.96056615139459,-3.17672322869252));
#9119=CARTESIAN_POINT('Ctrl Pts',(-3.12913513552178,7.84598281806096,-2.47412055785955));
#9120=CARTESIAN_POINT('Ctrl Pts',(-3.43949409635991,7.78869115139432,-2.04588554269906));
#9121=CARTESIAN_POINT('Ctrl Pts',(-3.87388118930893,7.67410781806122,-1.09803146582633));
#9122=CARTESIAN_POINT('Ctrl Pts',(-3.9977025943682,7.61681615139413,-0.578770475493801));
#9123=CARTESIAN_POINT('Ctrl Pts',(-4.03629588722871,7.50223281806141,0.472877455896854));
#9124=CARTESIAN_POINT('Ctrl Pts',(-3.95101381207413,7.44494115139464,1.00485064950196));
#9125=CARTESIAN_POINT('Ctrl Pts',(-3.58050442500531,7.33035781806089,2.00018857107951));
#9126=CARTESIAN_POINT('Ctrl Pts',(-3.29538705454006,7.27306615139411,2.46314686479214));
#9127=CARTESIAN_POINT('Ctrl Pts',(-2.56531411614172,7.15848281806142,3.24779896141502));
#9128=CARTESIAN_POINT('Ctrl Pts',(-2.12061835877177,7.10119115139444,3.5691566384858));
#9129=CARTESIAN_POINT('Ctrl Pts',(-1.13687264763148,6.98660781806109,4.01841053319279));
#9130=CARTESIAN_POINT('Ctrl Pts',(-0.598194887996293,6.92931615139405,4.14609417373796));
#9131=CARTESIAN_POINT('Ctrl Pts',(0.492301868399383,6.81473281806148,4.18468746665935));
#9132=CARTESIAN_POINT('Ctrl Pts',(1.04369183128993,6.75744115139454,4.09554315589853));
#9133=CARTESIAN_POINT('Ctrl Pts',(2.07492138716947,6.64285781806099,3.71016696719063));
#9134=CARTESIAN_POINT('Ctrl Pts',(2.55434042303921,6.585566151395,3.41405088038211));
#9135=CARTESIAN_POINT('Ctrl Pts',(3.36646278729771,6.47098281806054,2.65650767442937));
#9136=CARTESIAN_POINT('Ctrl Pts',(3.69881918061998,6.41369115139488,2.19535117483371));
#9137=CARTESIAN_POINT('Ctrl Pts',(4.16293987706837,6.29910781806065,1.1757138294474));
#9138=CARTESIAN_POINT('Ctrl Pts',(4.29448575311062,6.24181615139464,0.617619300488533));
#9139=CARTESIAN_POINT('Ctrl Pts',(4.3330790460871,6.1272328180609,-0.511726280891663));
#9140=CARTESIAN_POINT('Ctrl Pts',(4.24007249972198,6.06994115139421,-1.0825330130876));
#9141=CARTESIAN_POINT('Ctrl Pts',(3.8398295093769,5.95535781806132,-2.14965420324974));
#9142=CARTESIAN_POINT('Ctrl Pts',(3.53271470621635,5.89806615139432,-2.64553398129709));
#9143=CARTESIAN_POINT('Ctrl Pts',(2.74770123272482,5.78348281806122,-3.48512661316959));
#9144=CARTESIAN_POINT('Ctrl Pts',(2.27008399088731,5.72619115139493,-3.82848172276042));
#9145=CARTESIAN_POINT('Ctrl Pts',(1.21455501127165,5.6116078180606,-4.30746922093769));
#9146=CARTESIAN_POINT('Ctrl Pts',(0.637043712966868,5.55431615139431,-4.44287733248579));
#9147=CARTESIAN_POINT('Ctrl Pts',(-0.531150693370039,5.43973281806122,-4.48147062551234));
#9148=CARTESIAN_POINT('Ctrl Pts',(-1.12137419490063,5.38244115139481,-4.38460184354212));
#9149=CARTESIAN_POINT('Ctrl Pts',(-2.22438701931463,5.26785781806072,-3.96949205156649));
#9150=CARTESIAN_POINT('Ctrl Pts',(-2.73672753956158,5.21056615139485,-3.651378532048));
#9151=CARTESIAN_POINT('Ctrl Pts',(-3.60379043903486,5.09598281806069,-2.83889479102288));
#9152=CARTESIAN_POINT('Ctrl Pts',(-3.95814426490714,5.03869115139445,-2.34481680693236));
#9153=CARTESIAN_POINT('Ctrl Pts',(-4.45199856480073,4.92410781806109,-1.25339619310446));
#9154=CARTESIAN_POINT('Ctrl Pts',(-4.59126891186371,4.86681615139442,-0.656468125439367));
#9155=CARTESIAN_POINT('Ctrl Pts',(-4.62986220493482,4.75223281806112,0.550575105842595));
#9156=CARTESIAN_POINT('Ctrl Pts',(-4.52913118736181,4.69494115139439,1.1602153767205));
#9157=CARTESIAN_POINT('Ctrl Pts',(-4.09915459375653,4.58035781806114,2.2991198353727));
#9158=CARTESIAN_POINT('Ctrl Pts',(-3.77004235787144,4.52306615139435,2.82792109783747));
#9159=CARTESIAN_POINT('Ctrl Pts',(-2.93008834932913,4.40848281806118,3.72245426488873));
#9160=CARTESIAN_POINT('Ctrl Pts',(-2.41954962296883,4.35119115139434,4.08780680705904));
#9161=CARTESIAN_POINT('Ctrl Pts',(-1.29223737494584,4.2366078180612,4.59652790865858));
#9162=CARTESIAN_POINT('Ctrl Pts',(-0.675892537901207,4.17931615139434,4.73966049124289));
#9163=CARTESIAN_POINT('Ctrl Pts',(0.569999518304482,4.06473281806119,4.77825378435605));
#9164=CARTESIAN_POINT('Ctrl Pts',(1.19905655854802,4.00744115139456,4.67366053118015));
#9165=CARTESIAN_POINT('Ctrl Pts',(2.37385265142312,3.89285781806098,4.2288171359479));
#9166=CARTESIAN_POINT('Ctrl Pts',(2.91911465611821,3.83556615139452,3.88870618369294));
#9167=CARTESIAN_POINT('Ctrl Pts',(3.84111809073776,3.72098281806102,3.02128190763733));
#9168=CARTESIAN_POINT('Ctrl Pts',(4.21746934921548,3.66369115139447,2.49428243900129));
#9169=CARTESIAN_POINT('Ctrl Pts',(4.74105725251191,3.54910781806106,1.33107855679123));
#9170=CARTESIAN_POINT('Ctrl Pts',(4.88805207062498,3.49181615139418,0.695316950351842));
#9171=CARTESIAN_POINT('Ctrl Pts',(4.92664536377436,3.37723281806136,-0.589423930755165));
#9172=CARTESIAN_POINT('Ctrl Pts',(4.81818987499502,3.31994115139439,-1.23789774038871));
#9173=CARTESIAN_POINT('Ctrl Pts',(4.35847967814275,3.20535781806115,-2.44858546746038));
#9174=CARTESIAN_POINT('Ctrl Pts',(4.00737000950903,3.14806615139448,-3.01030821440669));
#9175=CARTESIAN_POINT('Ctrl Pts',(3.11247546595094,3.03348281806106,-3.95978191657904));
#9176=CARTESIAN_POINT('Ctrl Pts',(2.56901525502413,2.97619115139456,-4.34713189137729));
#9177=CARTESIAN_POINT('Ctrl Pts',(1.36991973864622,2.86160781806097,-4.88558659635986));
#9178=CARTESIAN_POINT('Ctrl Pts',(0.714741362801074,2.80431615139412,-5.0364436500079));
#9179=CARTESIAN_POINT('Ctrl Pts',(-0.608848343204429,2.68973281806141,-5.07503694319185));
#9180=CARTESIAN_POINT('Ctrl Pts',(-1.27673892223029,2.6324411513943,-4.96271921881159));
#9181=CARTESIAN_POINT('Ctrl Pts',(-2.52331828349673,2.51785781806124,-4.48814222033592));
#9182=CARTESIAN_POINT('Ctrl Pts',(-3.10150177270171,2.46056615139471,-4.12603383532024));
#9183=CARTESIAN_POINT('Ctrl Pts',(-4.0784457424138,2.34598281806081,-3.20366902426941));
#9184=CARTESIAN_POINT('Ctrl Pts',(-4.47679443354355,2.28869115139434,-2.64374807104099));
#9185=CARTESIAN_POINT('Ctrl Pts',(-5.03011594020335,2.1741078180612,-1.40876092050723));
#9186=CARTESIAN_POINT('Ctrl Pts',(-5.18483522939207,2.11681615139406,-0.734165775240769));
#9187=CARTESIAN_POINT('Ctrl Pts',(-5.22342852260808,2.00223281806147,0.628272755644193));
#9188=CARTESIAN_POINT('Ctrl Pts',(-5.10724856262497,1.94494115139452,1.31558010408276));
#9189=CARTESIAN_POINT('Ctrl Pts',(-4.61780476253225,1.83035781806102,2.59805109952221));
#9190=CARTESIAN_POINT('Ctrl Pts',(-4.24469766112837,1.77306615139441,3.1926953310021));
#9191=CARTESIAN_POINT('Ctrl Pts',(-3.29486258259099,1.65848281806113,4.19710956824316));
#9192=CARTESIAN_POINT('Ctrl Pts',(-2.71848088705236,1.60119115139435,4.60645697571289));
#9193=CARTESIAN_POINT('Ctrl Pts',(-1.44760210237368,1.48660781806119,5.17464528404378));
#9194=CARTESIAN_POINT('Ctrl Pts',(-0.753590187674045,1.42931615139403,5.33322680877775));
#9195=CARTESIAN_POINT('Ctrl Pts',(0.647697168077543,1.3147328180615,5.37182010202281));
#9196=CARTESIAN_POINT('Ctrl Pts',(1.35442128593412,1.25744115139439,5.25177790643984));
#9197=CARTESIAN_POINT('Ctrl Pts',(2.67278391554878,1.14285781806115,4.74746730472711));
#9198=CARTESIAN_POINT('Ctrl Pts',(3.28388888930855,1.08556615139459,4.36336148693201));
#9199=CARTESIAN_POINT('Ctrl Pts',(4.3157733940665,0.970982818060947,3.38605614091702));
#9200=CARTESIAN_POINT('Ctrl Pts',(4.73611951788435,0.913691151394175,2.79321370306255));
#9201=CARTESIAN_POINT('Ctrl Pts',(5.31917462788209,0.79910781806136,1.48644328424131));
#9202=CARTESIAN_POINT('Ctrl Pts',(5.48161838816491,0.741816151394642,0.773014600098004));
#9203=CARTESIAN_POINT('Ctrl Pts',(5.52021168143606,0.627232818060896,-0.667121580501539));
#9204=CARTESIAN_POINT('Ctrl Pts',(5.39630725025002,0.569941151394671,-1.39326246779836));
#9205=CARTESIAN_POINT('Ctrl Pts',(4.87712984692664,0.455357818060863,-2.7475167315625));
#9206=CARTESIAN_POINT('Ctrl Pts',(4.48202531273885,0.398066151394155,-3.37508244761294));
#9207=CARTESIAN_POINT('Ctrl Pts',(3.47724969923989,0.283482818061382,-4.43443721989186));
#9208=CARTESIAN_POINT('Ctrl Pts',(2.8679465190623,0.226191151394174,-4.86578206006134));
#9209=CARTESIAN_POINT('Ctrl Pts',(1.52528446611942,0.111607818061363,-5.46370397171486));
#9210=CARTESIAN_POINT('Ctrl Pts',(0.792439012521748,0.0543161513944402,
-5.63000996755282));
#9211=CARTESIAN_POINT('Ctrl Pts',(-0.686545992925361,-0.0602671819389035,
-5.66860326084855));
#9212=CARTESIAN_POINT('Ctrl Pts',(-1.43210364967231,-0.117558848605399,
-5.54083659405887));
#9213=CARTESIAN_POINT('Ctrl Pts',(-2.82224954756648,-0.232142181939065,
-5.00679238912752));
#9214=CARTESIAN_POINT('Ctrl Pts',(-3.46627599744854,-0.28943384860568,-4.6006891460729));
#9215=CARTESIAN_POINT('Ctrl Pts',(-4.0096885258173,-0.346725515272232,-4.08456619805421));
#9216=CARTESIAN_POINT('Ctrl Pts',(-2.36456791311707,11.0001838839337,-2.37391751282759));
#9217=CARTESIAN_POINT('Ctrl Pts',(-2.68439695740737,10.9428309226217,-2.07282384920463));
#9218=CARTESIAN_POINT('Ctrl Pts',(-2.94593475213736,10.885477961311,-1.70638527343931));
#9219=CARTESIAN_POINT('Ctrl Pts',(-3.30964371429254,10.7708333333336,-0.896538039613314));
#9220=CARTESIAN_POINT('Ctrl Pts',(-3.41180604852602,10.7135416666669,-0.453515668913589));
#9221=CARTESIAN_POINT('Ctrl Pts',(-3.4379002366457,10.5989583333331,0.443108774718904));
#9222=CARTESIAN_POINT('Ctrl Pts',(-3.36178304590245,10.5416666666666,0.896358100460257));
#9223=CARTESIAN_POINT('Ctrl Pts',(-3.03905091217473,10.4270833333334,1.74368979436799));
#9224=CARTESIAN_POINT('Ctrl Pts',(-2.79252711081109,10.3697916666664,2.13742396723561));
#9225=CARTESIAN_POINT('Ctrl Pts',(-2.16323413009096,10.2552083333337,2.80361970275416));
#9226=CARTESIAN_POINT('Ctrl Pts',(-1.78068510549046,10.1979166666664,3.07579175088966));
#9227=CARTESIAN_POINT('Ctrl Pts',(-0.935379221363662,10.0833333333336,3.45417305821104));
#9228=CARTESIAN_POINT('Ctrl Pts',(-0.472940081479242,10.0260416666666,3.56019762788479));
#9229=CARTESIAN_POINT('Ctrl Pts',(0.462533187284589,9.91145833333345,3.58629181608734));
#9230=CARTESIAN_POINT('Ctrl Pts',(0.935199282188079,9.85416666666669,3.50631238974053));
#9231=CARTESIAN_POINT('Ctrl Pts',(1.81842261051809,9.73958333333332,3.16871345434639));
#9232=CARTESIAN_POINT('Ctrl Pts',(2.22861752543397,9.68229166666673,2.91119093668731));
#9233=CARTESIAN_POINT('Ctrl Pts',(2.92228352868554,9.56770833333328,2.25442768834444));
#9234=CARTESIAN_POINT('Ctrl Pts',(3.20545429299277,9.51041666666666,1.85541792160244));
#9235=CARTESIAN_POINT('Ctrl Pts',(3.59870240211769,9.39583333333334,0.974220403129539));
#9236=CARTESIAN_POINT('Ctrl Pts',(3.70858920724845,9.3385416666664,0.492364494026195));
#9237=CARTESIAN_POINT('Ctrl Pts',(3.73468339552408,9.22395833333361,-0.481957599831572));
#9238=CARTESIAN_POINT('Ctrl Pts',(3.65084173357628,9.16666666666689,-0.974040463933888));
#9239=CARTESIAN_POINT('Ctrl Pts',(3.29837599652037,9.05208333333312,-1.8931554266502));
#9240=CARTESIAN_POINT('Ctrl Pts',(3.02985476255422,8.99479166666641,-2.31981108364774));
#9241=CARTESIAN_POINT('Ctrl Pts',(2.34562124660724,8.8802083333336,-3.04094735460153));
#9242=CARTESIAN_POINT('Ctrl Pts',(1.93015073770027,8.82291666666647,-3.33511683510577));
#9243=CARTESIAN_POINT('Ctrl Pts',(1.01306158490958,8.70833333333354,-3.74323174601444));
#9244=CARTESIAN_POINT('Ctrl Pts',(0.511788906557484,8.6510416666665,-3.85698078661577));
#9245=CARTESIAN_POINT('Ctrl Pts',(-0.501382012362897,8.53645833333351,-3.88307497495716));
#9246=CARTESIAN_POINT('Ctrl Pts',(-1.01288164569554,8.47916666666683,-3.79537107740945));
#9247=CARTESIAN_POINT('Ctrl Pts',(-1.96788824276646,8.36458333333318,-3.42803853869692));
#9248=CARTESIAN_POINT('Ctrl Pts',(-2.41100464187403,8.30729166666683,-3.14851858841386));
#9249=CARTESIAN_POINT('Ctrl Pts',(-3.159611180505,8.1927083333332,-2.43681480487731));
#9250=CARTESIAN_POINT('Ctrl Pts',(-3.46477937722837,8.13541666666656,-2.00488355378617));
#9251=CARTESIAN_POINT('Ctrl Pts',(-3.8877610899016,8.02083333333345,-1.05190276670153));
#9252=CARTESIAN_POINT('Ctrl Pts',(-4.00537236598643,7.96354166666637,-0.531213319073915));
#9253=CARTESIAN_POINT('Ctrl Pts',(-4.03146655438691,7.84895833333365,0.520806424879362));
#9254=CARTESIAN_POINT('Ctrl Pts',(-3.93990042124014,7.79166666666665,1.05172282747159));
#9255=CARTESIAN_POINT('Ctrl Pts',(-3.55770108087595,7.67708333333337,2.04262105886835));
#9256=CARTESIAN_POINT('Ctrl Pts',(-3.26718241426475,7.61979166666659,2.50219820011361));
#9257=CARTESIAN_POINT('Ctrl Pts',(-2.52800836315612,7.50520833333343,3.27827500639517));
#9258=CARTESIAN_POINT('Ctrl Pts',(-2.07961636986072,7.44791666666668,3.59444191935829));
#9259=CARTESIAN_POINT('Ctrl Pts',(-1.09074394850484,7.33333333333333,4.03229043378143));
#9260=CARTESIAN_POINT('Ctrl Pts',(-0.550637731576509,7.27604166666629,4.15376394536062));
#9261=CARTESIAN_POINT('Ctrl Pts',(0.540230837381994,7.16145833333372,4.17985813381312));
#9262=CARTESIAN_POINT('Ctrl Pts',(1.09056400926098,7.10416666666678,4.08442976506864));
#9263=CARTESIAN_POINT('Ctrl Pts',(2.11735387495688,6.98958333333323,3.68736362305719));
#9264=CARTESIAN_POINT('Ctrl Pts',(2.59339175836345,6.93229166666724,3.38584624010982));
#9265=CARTESIAN_POINT('Ctrl Pts',(3.3969388322751,6.81770833333277,2.61920192144075));
#9266=CARTESIAN_POINT('Ctrl Pts',(3.72410446149635,6.76041666666712,2.15434918592434));
#9267=CARTESIAN_POINT('Ctrl Pts',(4.17681977765313,6.64583333333289,1.12958513031907));
#9268=CARTESIAN_POINT('Ctrl Pts',(4.30215552473732,6.58854166666688,0.570062144068889));
#9269=CARTESIAN_POINT('Ctrl Pts',(4.32824971323683,6.47395833333313,-0.559655249874413));
#9270=CARTESIAN_POINT('Ctrl Pts',(4.22895910889563,6.41666666666645,-1.12940519106012));
#9271=CARTESIAN_POINT('Ctrl Pts',(3.81702616523991,6.30208333333356,-2.19208669103568));
#9272=CARTESIAN_POINT('Ctrl Pts',(3.50451006594675,6.24479166666656,-2.68458531662391));
#9273=CARTESIAN_POINT('Ctrl Pts',(2.71039547973352,6.13020833333345,-3.51560265814439));
#9274=CARTESIAN_POINT('Ctrl Pts',(2.22908200197935,6.07291666666717,-3.85376700363998));
#9275=CARTESIAN_POINT('Ctrl Pts',(1.16842631214193,5.95833333333284,-4.32134912151925));
#9276=CARTESIAN_POINT('Ctrl Pts',(0.589486556547344,5.90104166666655,-4.45054710411593));
#9277=CARTESIAN_POINT('Ctrl Pts',(-0.579079662352908,5.78645833333346,-4.47664129265863));
#9278=CARTESIAN_POINT('Ctrl Pts',(-1.16824637287424,5.72916666666705,-4.37348845271886));
#9279=CARTESIAN_POINT('Ctrl Pts',(-2.26681950709949,5.61458333333296,-3.94668870742641));
#9280=CARTESIAN_POINT('Ctrl Pts',(-2.77577887489086,5.55729166666709,-3.62317389178086));
#9281=CARTESIAN_POINT('Ctrl Pts',(-3.6342664840072,5.44270833333292,-2.80158903802911));
#9282=CARTESIAN_POINT('Ctrl Pts',(-3.98342954578962,5.38541666666669,-2.30381481802579));
#9283=CARTESIAN_POINT('Ctrl Pts',(-4.46587846537937,5.27083333333332,-1.20726749397333));
#9284=CARTESIAN_POINT('Ctrl Pts',(-4.59893868349712,5.21354166666665,-0.608910969019916));
#9285=CARTESIAN_POINT('Ctrl Pts',(-4.62503287207784,5.09895833333335,0.598504074825539));
#9286=CARTESIAN_POINT('Ctrl Pts',(-4.51801779654147,5.04166666666663,1.20708755469526));
#9287=CARTESIAN_POINT('Ctrl Pts',(-4.07635124961353,4.92708333333338,2.34155232315641));
#9288=CARTESIAN_POINT('Ctrl Pts',(-3.74183771760646,4.86979166666659,2.86697243316876));
#9289=CARTESIAN_POINT('Ctrl Pts',(-2.89278259633321,4.75520833333342,3.75293030985906));
#9290=CARTESIAN_POINT('Ctrl Pts',(-2.37854763406351,4.69791666666658,4.1130920879442));
#9291=CARTESIAN_POINT('Ctrl Pts',(-1.24610867581347,4.58333333333343,4.61040780923455));
#9292=CARTESIAN_POINT('Ctrl Pts',(-0.628335381481812,4.52604166666658,4.74733026287932));
#9293=CARTESIAN_POINT('Ctrl Pts',(0.617928487287482,4.41145833333343,4.77342445149605));
#9294=CARTESIAN_POINT('Ctrl Pts',(1.24592873652376,4.35416666666679,4.66254714036264));
#9295=CARTESIAN_POINT('Ctrl Pts',(2.41628513920584,4.23958333333322,4.20601379180208));
#9296=CARTESIAN_POINT('Ctrl Pts',(2.95816599145146,4.18229166666676,3.86050154342994));
#9297=CARTESIAN_POINT('Ctrl Pts',(3.87159413570613,4.06770833333325,2.98397615463943));
#9298=CARTESIAN_POINT('Ctrl Pts',(4.24275463010319,4.01041666666671,2.45328045009706));
#9299=CARTESIAN_POINT('Ctrl Pts',(4.75493715308532,3.8958333333333,1.28494985765777));
#9300=CARTESIAN_POINT('Ctrl Pts',(4.89572184226387,3.83854166666642,0.647759793932574));
#9301=CARTESIAN_POINT('Ctrl Pts',(4.9218160309119,3.72395833333359,-0.637352899738291));
#9302=CARTESIAN_POINT('Ctrl Pts',(4.80707648417982,3.66666666666662,-1.28476991836542));
#9303=CARTESIAN_POINT('Ctrl Pts',(4.33567633399462,3.55208333333339,-2.49101795524214));
#9304=CARTESIAN_POINT('Ctrl Pts',(3.97916536924807,3.49479166666671,-3.04935954974168));
#9305=CARTESIAN_POINT('Ctrl Pts',(3.075169712951,3.38020833333329,-3.99025796154567));
#9306=CARTESIAN_POINT('Ctrl Pts',(2.52801326612096,3.3229166666668,-4.37241717226731));
#9307=CARTESIAN_POINT('Ctrl Pts',(1.3237910395117,3.20833333333321,-4.89946649693097));
#9308=CARTESIAN_POINT('Ctrl Pts',(0.667184206381905,3.15104166666636,-5.04411342164931));
#9309=CARTESIAN_POINT('Ctrl Pts',(-0.656777312187654,3.03645833333365,-5.07020761032686));
#9310=CARTESIAN_POINT('Ctrl Pts',(-1.32361110020785,2.97916666666654,-4.95160582799841));
#9311=CARTESIAN_POINT('Ctrl Pts',(-2.56575077127763,2.86458333333347,-4.46533887618575));
#9312=CARTESIAN_POINT('Ctrl Pts',(-3.1405531080382,2.80729166666695,-4.09782919506089));
#9313=CARTESIAN_POINT('Ctrl Pts',(-4.10892178737893,2.69270833333305,-3.16636327126786));
#9314=CARTESIAN_POINT('Ctrl Pts',(-4.50207971443576,2.63541666666658,-2.60274608213879));
#9315=CARTESIAN_POINT('Ctrl Pts',(-5.04399584077227,2.52083333333343,-1.36263222137173));
#9316=CARTESIAN_POINT('Ctrl Pts',(-5.1925050010359,2.4635416666663,-0.686608618821642));
#9317=CARTESIAN_POINT('Ctrl Pts',(-5.21859918974068,2.34895833333371,0.67620172462746));
#9318=CARTESIAN_POINT('Ctrl Pts',(-5.09613517181383,2.29166666666676,1.36245228206106));
#9319=CARTESIAN_POINT('Ctrl Pts',(-4.59500141838005,2.17708333333325,2.64048358730238));
#9320=CARTESIAN_POINT('Ctrl Pts',(-4.21649302087059,2.11979166666664,3.23174666634004));
#9321=CARTESIAN_POINT('Ctrl Pts',(-3.25755682958786,2.00520833333337,4.22758561320685));
#9322=CARTESIAN_POINT('Ctrl Pts',(-2.67747889815098,1.94791666666658,4.63174225660692));
#9323=CARTESIAN_POINT('Ctrl Pts',(-1.40147340323737,1.83333333333343,5.18852518461089));
#9324=CARTESIAN_POINT('Ctrl Pts',(-0.706033031254986,1.77604166666627,5.34089658042353));
#9325=CARTESIAN_POINT('Ctrl Pts',(0.695626137060878,1.66145833333374,5.36699076915345));
#9326=CARTESIAN_POINT('Ctrl Pts',(1.40129346391331,1.60416666666663,5.24066451563091));
#9327=CARTESIAN_POINT('Ctrl Pts',(2.71521640332806,1.48958333333338,4.7246639605727));
#9328=CARTESIAN_POINT('Ctrl Pts',(3.32294022464786,1.43229166666683,4.33515684667557));
#9329=CARTESIAN_POINT('Ctrl Pts',(4.34624943902881,1.31770833333318,3.34875038791256));
#9330=CARTESIAN_POINT('Ctrl Pts',(4.76140479878007,1.26041666666641,2.75221171416214));
#9331=CARTESIAN_POINT('Ctrl Pts',(5.3330545284475,1.1458333333336,1.44031458510402));
#9332=CARTESIAN_POINT('Ctrl Pts',(5.48928815981245,1.08854166666688,0.72545744367903));
#9333=CARTESIAN_POINT('Ctrl Pts',(5.51538234856494,0.973958333333134,-0.715050549484959));
#9334=CARTESIAN_POINT('Ctrl Pts',(5.38519385944284,0.916666666666909,-1.44013464577813));
#9335=CARTESIAN_POINT('Ctrl Pts',(4.85432650277048,0.8020833333331,-2.7899492193412));
#9336=CARTESIAN_POINT('Ctrl Pts',(4.4538206724838,0.744791666666392,-3.4141337829535));
#9337=CARTESIAN_POINT('Ctrl Pts',(3.43994394623404,0.630208333333619,-4.46491326485293));
#9338=CARTESIAN_POINT('Ctrl Pts',(2.82694453016243,0.572916666666411,-4.89106734095877));
#9339=CARTESIAN_POINT('Ctrl Pts',(1.47915576698159,0.4583333333336,-5.47758387227856));
#9340=CARTESIAN_POINT('Ctrl Pts',(0.744881856102772,0.401041666666677,-5.63767973920226));
#9341=CARTESIAN_POINT('Ctrl Pts',(-0.73447496190878,0.286458333333334,-5.66377392797554));
#9342=CARTESIAN_POINT('Ctrl Pts',(-1.4789758276525,0.229166666666838,-5.52972320325324));
#9343=CARTESIAN_POINT('Ctrl Pts',(-2.86468203534475,0.114583333333173,-4.9839890449698));
#9344=CARTESIAN_POINT('Ctrl Pts',(-3.50532733285514,0.0572916666665569,
-4.5724845058884));
#9345=CARTESIAN_POINT('Ctrl Pts',(-4.04445221596811,5.20417042793042E-15,
-4.05181100142375));
#9346=CARTESIAN_POINT('',(-3.80443305520312,5.15793290147402E-15,-3.79707426974638));
#9347=CARTESIAN_POINT('Ctrl Pts',(-2.45534485149915,10.9282219455009,-1.7516666854678));
#9348=CARTESIAN_POINT('Ctrl Pts',(-2.59470810356228,10.8948562970005,-1.56864042896568));
#9349=CARTESIAN_POINT('Ctrl Pts',(-2.71374107587765,10.8614906485003,-1.3691084593084));
#9350=CARTESIAN_POINT('Ctrl Pts',(-2.97162798586693,10.7708333333336,-0.794830755283512));
#9351=CARTESIAN_POINT('Ctrl Pts',(-3.06332306119362,10.7135416666669,-0.397314139662748));
#9352=CARTESIAN_POINT('Ctrl Pts',(-3.08669273082211,10.5989583333331,0.407721033857582));
#9353=CARTESIAN_POINT('Ctrl Pts',(-3.01831935235521,10.5416666666666,0.814922877330024));
#9354=CARTESIAN_POINT('Ctrl Pts',(-2.728119788021,10.4270833333334,1.57659449107116));
#9355=CARTESIAN_POINT('Ctrl Pts',(-2.50637194487625,10.3697916666664,1.93074976622997));
#9356=CARTESIAN_POINT('Ctrl Pts',(-1.93991583267103,10.2552083333337,2.53025558222984));
#9357=CARTESIAN_POINT('Ctrl Pts',(-1.59540299717169,10.1979166666664,2.77534284559852));
#9358=CARTESIAN_POINT('Ctrl Pts',(-0.833671937081177,10.0833333333336,3.11615732976406));
#9359=CARTESIAN_POINT('Ctrl Pts',(-0.416738552178117,10.0260416666666,3.21171464055396));
#9360=CARTESIAN_POINT('Ctrl Pts',(0.427145446372979,9.91145833333345,3.23508431026218));
#9361=CARTESIAN_POINT('Ctrl Pts',(0.853764059103477,9.85416666666669,3.16284869617602));
#9362=CARTESIAN_POINT('Ctrl Pts',(1.65132730717562,9.73958333333332,2.85778233020993));
#9363=CARTESIAN_POINT('Ctrl Pts',(2.02194332446279,9.68229166666673,2.62503577071995));
#9364=CARTESIAN_POINT('Ctrl Pts',(2.64891940812677,9.56770833333328,2.03110939095704));
#9365=CARTESIAN_POINT('Ctrl Pts',(2.9050053877204,9.51041666666666,1.67013581324179));
#9366=CARTESIAN_POINT('Ctrl Pts',(3.26068667365192,9.39583333333334,0.872513118888943));
#9367=CARTESIAN_POINT('Ctrl Pts',(3.36010621991895,9.3385416666664,0.436162964680591));
#9368=CARTESIAN_POINT('Ctrl Pts',(3.38347588969759,9.22395833333361,-0.446569858875482));
#9369=CARTESIAN_POINT('Ctrl Pts',(3.30737803999626,9.16666666666689,-0.892605240889856));
#9370=CARTESIAN_POINT('Ctrl Pts',(2.98744487239941,9.05208333333312,-1.72606012326716));
#9371=CARTESIAN_POINT('Ctrl Pts',(2.74369959655829,8.99479166666641,-2.11313688270712));
#9372=CARTESIAN_POINT('Ctrl Pts',(2.1223029492484,8.8802083333336,-2.76758323401219));
#9373=CARTESIAN_POINT('Ctrl Pts',(1.74486862930228,8.82291666666647,-3.03466792985017));
#9374=CARTESIAN_POINT('Ctrl Pts',(0.911354300706321,8.70833333333354,-3.40521601753191));
#9375=CARTESIAN_POINT('Ctrl Pts',(0.455587377172263,8.6510416666665,-3.5084977992874));
#9376=CARTESIAN_POINT('Ctrl Pts',(-0.465994271367186,8.53645833333351,-3.53186746912954));
#9377=CARTESIAN_POINT('Ctrl Pts',(-0.93144642268745,8.47916666666683,-3.45190738381581));
#9378=CARTESIAN_POINT('Ctrl Pts',(-1.80079293934749,8.36458333333318,-3.11710741458959));
#9379=CARTESIAN_POINT('Ctrl Pts',(-2.20433044096071,8.30729166666683,-2.86236342239196));
#9380=CARTESIAN_POINT('Ctrl Pts',(-2.88624705988836,8.1927083333332,-2.21349650754444));
#9381=CARTESIAN_POINT('Ctrl Pts',(-3.1643304719878,8.13541666666656,-1.81960144535507));
#9382=CARTESIAN_POINT('Ctrl Pts',(-3.54974536140404,8.02083333333345,-0.950195482531384));
#9383=CARTESIAN_POINT('Ctrl Pts',(-3.65688937865929,7.96354166666637,-0.475011789653154));
#9384=CARTESIAN_POINT('Ctrl Pts',(-3.68025904855805,7.84895833333365,0.485418683848109));
#9385=CARTESIAN_POINT('Ctrl Pts',(-3.59643672763413,7.79166666666665,0.970287604495667));
#9386=CARTESIAN_POINT('Ctrl Pts',(-3.246769956781,7.67708333333337,1.8755257554172));
#9387=CARTESIAN_POINT('Ctrl Pts',(-2.98102724821984,7.61979166666659,2.29552399922486));
#9388=CARTESIAN_POINT('Ctrl Pts',(-2.30469006584627,7.50520833333343,3.00491088575395));
#9389=CARTESIAN_POINT('Ctrl Pts',(-1.89433426139971,7.44791666666668,3.29399301413121));
#9390=CARTESIAN_POINT('Ctrl Pts',(-0.989036664364609,7.33333333333333,3.69427470527038));
#9391=CARTESIAN_POINT('Ctrl Pts',(-0.49443620212397,7.27604166666629,3.80528095803426));
#9392=CARTESIAN_POINT('Ctrl Pts',(0.50484309631896,7.16145833333372,3.82865062798349));
#9393=CARTESIAN_POINT('Ctrl Pts',(1.00912878631411,7.10416666666678,3.74096607145172));
#9394=CARTESIAN_POINT('Ctrl Pts',(1.95025857147667,6.98958333333323,3.37643249897315));
#9395=CARTESIAN_POINT('Ctrl Pts',(2.38671755749636,6.93229166666724,3.09969107404422));
#9396=CARTESIAN_POINT('Ctrl Pts',(3.12357471161222,6.81770833333277,2.39588362415159));
#9397=CARTESIAN_POINT('Ctrl Pts',(3.42365555628099,6.76041666666712,1.96906707743673));
#9398=CARTESIAN_POINT('Ctrl Pts',(3.83880404913035,6.64583333333289,1.02787784620545));
#9399=CARTESIAN_POINT('Ctrl Pts',(3.95367253741186,6.58854166666688,0.51386061458762));
#9400=CARTESIAN_POINT('Ctrl Pts',(3.97704220740629,6.47395833333313,-0.524267508782646));
#9401=CARTESIAN_POINT('Ctrl Pts',(3.88549541526866,6.41666666666645,-1.04796996813959));
#9402=CARTESIAN_POINT('Ctrl Pts',(3.50609504116593,6.30208333333356,-2.02499138752914));
#9403=CARTESIAN_POINT('Ctrl Pts',(3.2183548998624,6.24479166666656,-2.47791111577681));
#9404=CARTESIAN_POINT('Ctrl Pts',(2.48707718246311,6.13020833333345,-3.24223853746153));
#9405=CARTESIAN_POINT('Ctrl Pts',(2.04379989346725,6.07291666666717,-3.55331809843599));
#9406=CARTESIAN_POINT('Ctrl Pts',(1.06671902805278,5.95833333333284,-3.9833333929851));
#9407=CARTESIAN_POINT('Ctrl Pts',(0.533285027040294,5.90104166666655,-4.10206411679133));
#9408=CARTESIAN_POINT('Ctrl Pts',(-0.543691921235359,5.78645833333346,-4.12543378682723));
#9409=CARTESIAN_POINT('Ctrl Pts',(-1.08681114997705,5.72916666666705,-4.03002475908303));
#9410=CARTESIAN_POINT('Ctrl Pts',(-2.0997242035696,5.61458333333296,-3.63575758336128));
#9411=CARTESIAN_POINT('Ctrl Pts',(-2.56910467406188,5.55729166666709,-3.33701872567955));
#9412=CARTESIAN_POINT('Ctrl Pts',(-3.36090236330622,5.44270833333292,-2.57827074077566));
#9413=CARTESIAN_POINT('Ctrl Pts',(-3.68298064059524,5.38541666666669,-2.11853270949184));
#9414=CARTESIAN_POINT('Ctrl Pts',(-4.12786273683561,5.27083333333332,-1.10556020990605));
#9415=CARTESIAN_POINT('Ctrl Pts',(-4.25045569617289,5.21354166666665,-0.552709439489368));
#9416=CARTESIAN_POINT('Ctrl Pts',(-4.27382536624608,5.09895833333335,0.563116333684488));
#9417=CARTESIAN_POINT('Ctrl Pts',(-4.17455410289751,5.04166666666663,1.12565233181968));
#9418=CARTESIAN_POINT('Ctrl Pts',(-3.76542012555652,4.92708333333338,2.17445701960491));
#9419=CARTESIAN_POINT('Ctrl Pts',(-3.45568255149002,4.86979166666659,2.66029823235588));
#9420=CARTESIAN_POINT('Ctrl Pts',(-2.6694642990949,4.75520833333342,3.47956618914197));
#9421=CARTESIAN_POINT('Ctrl Pts',(-2.19326552550957,4.69791666666658,3.81264318275876));
#9422=CARTESIAN_POINT('Ctrl Pts',(-1.14440139176617,4.58333333333343,4.27239208068185));
#9423=CARTESIAN_POINT('Ctrl Pts',(-0.572133851929879,4.52604166666658,4.39884727555618));
#9424=CARTESIAN_POINT('Ctrl Pts',(0.582540746125043,4.41145833333343,4.42221694566319));
#9425=CARTESIAN_POINT('Ctrl Pts',(1.16449351366757,4.35416666666679,4.31908344671154));
#9426=CARTESIAN_POINT('Ctrl Pts',(2.24918983563495,4.23958333333322,3.89508266775222));
#9427=CARTESIAN_POINT('Ctrl Pts',(2.75149179065353,4.18229166666676,3.57434637729919));
#9428=CARTESIAN_POINT('Ctrl Pts',(3.59823001497408,4.06770833333325,2.76065785741543));
#9429=CARTESIAN_POINT('Ctrl Pts',(3.94230572492611,4.01041666666671,2.26799834152485));
#9430=CARTESIAN_POINT('Ctrl Pts',(4.41692142452426,3.8958333333333,1.18324257362874));
#9431=CARTESIAN_POINT('Ctrl Pts',(4.54723885494094,3.83854166666642,0.591558264361257));
#9432=CARTESIAN_POINT('Ctrl Pts',(4.57060852507883,3.72395833333359,-0.601965158556466));
#9433=CARTESIAN_POINT('Ctrl Pts',(4.46361279052205,3.66666666666662,-1.20333469552689));
#9434=CARTESIAN_POINT('Ctrl Pts',(4.02474520995143,3.55208333333339,-2.32392265165357));
#9435=CARTESIAN_POINT('Ctrl Pts',(3.69301020310442,3.49479166666671,-2.84268534895739));
#9436=CARTESIAN_POINT('Ctrl Pts',(2.85185141573989,3.38020833333329,-3.71689384079999));
#9437=CARTESIAN_POINT('Ctrl Pts',(2.34273115753217,3.3229166666668,-4.07196826709743));
#9438=CARTESIAN_POINT('Ctrl Pts',(1.22208375549926,3.20833333333321,-4.56145076836271));
#9439=CARTESIAN_POINT('Ctrl Pts',(0.610982676792531,3.15104166666636,-4.6956304343271));
#9440=CARTESIAN_POINT('Ctrl Pts',(-0.621389570987771,3.03645833333365,-4.71900010449308));
#9441=CARTESIAN_POINT('Ctrl Pts',(-1.24217587738614,2.97916666666654,-4.60814213433379));
#9442=CARTESIAN_POINT('Ctrl Pts',(-2.39865546767225,2.86458333333347,-4.15440775214941));
#9443=CARTESIAN_POINT('Ctrl Pts',(-2.93387890726637,2.80729166666695,-3.81167402890586));
#9444=CARTESIAN_POINT('Ctrl Pts',(-3.83555766662078,2.69270833333305,-2.94304497406814));
#9445=CARTESIAN_POINT('Ctrl Pts',(-4.20163080927273,2.63541666666658,-2.41746397353493));
#9446=CARTESIAN_POINT('Ctrl Pts',(-4.70598011219716,2.52083333333343,-1.26092493737436));
#9447=CARTESIAN_POINT('Ctrl Pts',(-4.84402201371418,2.4635416666663,-0.630407089215845));
#9448=CARTESIAN_POINT('Ctrl Pts',(-4.86739168390641,2.34895833333371,0.64081398341115));
#9449=CARTESIAN_POINT('Ctrl Pts',(-4.75267147814405,2.29166666666676,1.28101705925391));
#9450=CARTESIAN_POINT('Ctrl Pts',(-4.28407029434887,2.17708333333325,2.47338828368244));
#9451=CARTESIAN_POINT('Ctrl Pts',(-3.93033785470491,2.11979166666664,3.0250724655795));
#9452=CARTESIAN_POINT('Ctrl Pts',(-3.0342385323988,2.00520833333337,3.95422149243741));
#9453=CARTESIAN_POINT('Ctrl Pts',(-2.49219678953305,1.94791666666658,4.33129335145034));
#9454=CARTESIAN_POINT('Ctrl Pts',(-1.29976611925407,1.83333333333343,4.85050945602931));
#9455=CARTESIAN_POINT('Ctrl Pts',(-0.6498315016342,1.77604166666627,4.99241359310244));
#9456=CARTESIAN_POINT('Ctrl Pts',(0.660238395829575,1.66145833333374,5.01578326331855));
#9457=CARTESIAN_POINT('Ctrl Pts',(1.31985824112059,1.60416666666663,4.89720082195578));
#9458=CARTESIAN_POINT('Ctrl Pts',(2.54812109969368,1.48958333333338,4.41373283654687));
#9459=CARTESIAN_POINT('Ctrl Pts',(3.1162660238978,1.43229166666683,4.04900168050008));
#9460=CARTESIAN_POINT('Ctrl Pts',(4.07288531824889,1.31770833333318,3.1254320907333));
#9461=CARTESIAN_POINT('Ctrl Pts',(4.460955893629,1.26041666666641,2.56692960553103));
#9462=CARTESIAN_POINT('Ctrl Pts',(4.99503879986042,1.1458333333336,1.33860730113391));
#9463=CARTESIAN_POINT('Ctrl Pts',(5.14080517249185,1.08854166666688,0.669255914044516));
#9464=CARTESIAN_POINT('Ctrl Pts',(5.16417484272955,0.973958333333134,-0.679662808239928));
#9465=CARTESIAN_POINT('Ctrl Pts',(5.04173016576313,0.916666666666909,-1.35869942299763));
#9466=CARTESIAN_POINT('Ctrl Pts',(4.54339537874923,0.8020833333331,-2.62285391569459));
#9467=CARTESIAN_POINT('Ctrl Pts',(4.16766550629842,0.744791666666392,-3.20745958221381));
#9468=CARTESIAN_POINT('Ctrl Pts',(3.21662564906467,0.630208333333619,-4.19154914406263));
#9469=CARTESIAN_POINT('Ctrl Pts',(2.6416624215197,0.572916666666411,-4.59061843581319));
#9470=CARTESIAN_POINT('Ctrl Pts',(1.3774484830231,0.4583333333336,-5.13956814368599));
#9471=CARTESIAN_POINT('Ctrl Pts',(0.688680326455284,0.401041666666677,-5.28919675188146));
#9472=CARTESIAN_POINT('Ctrl Pts',(-0.69908722065077,0.286458333333334,-5.31256642214034));
#9473=CARTESIAN_POINT('Ctrl Pts',(-1.39754060488348,0.229166666666838,-5.1862595095691));
#9474=CARTESIAN_POINT('Ctrl Pts',(-2.69758673168668,0.114583333333173,-4.67305792095299));
#9475=CARTESIAN_POINT('Ctrl Pts',(-3.29865313262765,0.0572916666665569,
-4.28632933922004));
#9476=CARTESIAN_POINT('Ctrl Pts',(-3.80443305520312,5.15793290147402E-15,
-3.79707426974638));
#9477=CARTESIAN_POINT('',(-4.04445221596811,5.20417042793042E-15,-4.05181100142375));
#9478=CARTESIAN_POINT('Origin',(-3.92444263558561,5.20417042793042E-15,
-3.92444263558507));
#9479=CARTESIAN_POINT('Ctrl Pts',(-2.3674783363584,10.9996616868026,-2.37117425835928));
#9480=CARTESIAN_POINT('Ctrl Pts',(-2.68598375393219,10.9424827912009,-2.07059921730022));
#9481=CARTESIAN_POINT('Ctrl Pts',(-2.94648697390286,10.8853038956006,-1.70515567693283));
#9482=CARTESIAN_POINT('Ctrl Pts',(-3.30964371429254,10.7708333333336,-0.896538039613314));
#9483=CARTESIAN_POINT('Ctrl Pts',(-3.41180604852602,10.7135416666669,-0.453515668913589));
#9484=CARTESIAN_POINT('Ctrl Pts',(-3.4379002366457,10.5989583333331,0.443108774718904));
#9485=CARTESIAN_POINT('Ctrl Pts',(-3.36178304590245,10.5416666666666,0.896358100460257));
#9486=CARTESIAN_POINT('Ctrl Pts',(-3.03905091217473,10.4270833333334,1.74368979436799));
#9487=CARTESIAN_POINT('Ctrl Pts',(-2.79252711081109,10.3697916666664,2.13742396723561));
#9488=CARTESIAN_POINT('Ctrl Pts',(-2.16323413009096,10.2552083333337,2.80361970275416));
#9489=CARTESIAN_POINT('Ctrl Pts',(-1.78068510549046,10.1979166666664,3.07579175088966));
#9490=CARTESIAN_POINT('Ctrl Pts',(-0.935379221363662,10.0833333333336,3.45417305821104));
#9491=CARTESIAN_POINT('Ctrl Pts',(-0.472940081479242,10.0260416666666,3.56019762788479));
#9492=CARTESIAN_POINT('Ctrl Pts',(0.462533187284589,9.91145833333345,3.58629181608734));
#9493=CARTESIAN_POINT('Ctrl Pts',(0.935199282188079,9.85416666666669,3.50631238974053));
#9494=CARTESIAN_POINT('Ctrl Pts',(1.81842261051809,9.73958333333332,3.16871345434639));
#9495=CARTESIAN_POINT('Ctrl Pts',(2.22861752543397,9.68229166666673,2.91119093668731));
#9496=CARTESIAN_POINT('Ctrl Pts',(2.92228352868554,9.56770833333328,2.25442768834444));
#9497=CARTESIAN_POINT('Ctrl Pts',(3.20545429299277,9.51041666666666,1.85541792160244));
#9498=CARTESIAN_POINT('Ctrl Pts',(3.59870240211769,9.39583333333334,0.974220403129539));
#9499=CARTESIAN_POINT('Ctrl Pts',(3.70858920724845,9.3385416666664,0.492364494026195));
#9500=CARTESIAN_POINT('Ctrl Pts',(3.73468339552408,9.22395833333361,-0.481957599831572));
#9501=CARTESIAN_POINT('Ctrl Pts',(3.65084173357628,9.16666666666689,-0.974040463933888));
#9502=CARTESIAN_POINT('Ctrl Pts',(3.29837599652037,9.05208333333312,-1.8931554266502));
#9503=CARTESIAN_POINT('Ctrl Pts',(3.02985476255422,8.99479166666641,-2.31981108364774));
#9504=CARTESIAN_POINT('Ctrl Pts',(2.34562124660724,8.8802083333336,-3.04094735460153));
#9505=CARTESIAN_POINT('Ctrl Pts',(1.93015073770027,8.82291666666647,-3.33511683510577));
#9506=CARTESIAN_POINT('Ctrl Pts',(1.01306158490958,8.70833333333354,-3.74323174601444));
#9507=CARTESIAN_POINT('Ctrl Pts',(0.511788906557484,8.6510416666665,-3.85698078661577));
#9508=CARTESIAN_POINT('Ctrl Pts',(-0.501382012362897,8.53645833333351,-3.88307497495716));
#9509=CARTESIAN_POINT('Ctrl Pts',(-1.01288164569554,8.47916666666683,-3.79537107740945));
#9510=CARTESIAN_POINT('Ctrl Pts',(-1.96788824276646,8.36458333333318,-3.42803853869692));
#9511=CARTESIAN_POINT('Ctrl Pts',(-2.41100464187403,8.30729166666683,-3.14851858841386));
#9512=CARTESIAN_POINT('Ctrl Pts',(-3.159611180505,8.1927083333332,-2.43681480487731));
#9513=CARTESIAN_POINT('Ctrl Pts',(-3.46477937722837,8.13541666666656,-2.00488355378617));
#9514=CARTESIAN_POINT('Ctrl Pts',(-3.8877610899016,8.02083333333345,-1.05190276670153));
#9515=CARTESIAN_POINT('Ctrl Pts',(-4.00537236598643,7.96354166666637,-0.531213319073915));
#9516=CARTESIAN_POINT('Ctrl Pts',(-4.03146655438691,7.84895833333365,0.520806424879362));
#9517=CARTESIAN_POINT('Ctrl Pts',(-3.93990042124014,7.79166666666665,1.05172282747159));
#9518=CARTESIAN_POINT('Ctrl Pts',(-3.55770108087595,7.67708333333337,2.04262105886835));
#9519=CARTESIAN_POINT('Ctrl Pts',(-3.26718241426475,7.61979166666659,2.50219820011361));
#9520=CARTESIAN_POINT('Ctrl Pts',(-2.52800836315612,7.50520833333343,3.27827500639517));
#9521=CARTESIAN_POINT('Ctrl Pts',(-2.07961636986072,7.44791666666668,3.59444191935829));
#9522=CARTESIAN_POINT('Ctrl Pts',(-1.09074394850484,7.33333333333333,4.03229043378143));
#9523=CARTESIAN_POINT('Ctrl Pts',(-0.550637731576509,7.27604166666629,4.15376394536062));
#9524=CARTESIAN_POINT('Ctrl Pts',(0.540230837381994,7.16145833333372,4.17985813381312));
#9525=CARTESIAN_POINT('Ctrl Pts',(1.09056400926098,7.10416666666678,4.08442976506864));
#9526=CARTESIAN_POINT('Ctrl Pts',(2.11735387495688,6.98958333333323,3.68736362305719));
#9527=CARTESIAN_POINT('Ctrl Pts',(2.59339175836345,6.93229166666724,3.38584624010982));
#9528=CARTESIAN_POINT('Ctrl Pts',(3.3969388322751,6.81770833333277,2.61920192144075));
#9529=CARTESIAN_POINT('Ctrl Pts',(3.72410446149635,6.76041666666712,2.15434918592434));
#9530=CARTESIAN_POINT('Ctrl Pts',(4.17681977765313,6.64583333333289,1.12958513031907));
#9531=CARTESIAN_POINT('Ctrl Pts',(4.30215552473732,6.58854166666688,0.570062144068889));
#9532=CARTESIAN_POINT('Ctrl Pts',(4.32824971323683,6.47395833333313,-0.559655249874413));
#9533=CARTESIAN_POINT('Ctrl Pts',(4.22895910889563,6.41666666666645,-1.12940519106012));
#9534=CARTESIAN_POINT('Ctrl Pts',(3.81702616523991,6.30208333333356,-2.19208669103568));
#9535=CARTESIAN_POINT('Ctrl Pts',(3.50451006594675,6.24479166666656,-2.68458531662391));
#9536=CARTESIAN_POINT('Ctrl Pts',(2.71039547973352,6.13020833333345,-3.51560265814439));
#9537=CARTESIAN_POINT('Ctrl Pts',(2.22908200197935,6.07291666666717,-3.85376700363998));
#9538=CARTESIAN_POINT('Ctrl Pts',(1.16842631214193,5.95833333333284,-4.32134912151925));
#9539=CARTESIAN_POINT('Ctrl Pts',(0.589486556547344,5.90104166666655,-4.45054710411593));
#9540=CARTESIAN_POINT('Ctrl Pts',(-0.579079662352908,5.78645833333346,-4.47664129265863));
#9541=CARTESIAN_POINT('Ctrl Pts',(-1.16824637287424,5.72916666666705,-4.37348845271886));
#9542=CARTESIAN_POINT('Ctrl Pts',(-2.26681950709949,5.61458333333296,-3.94668870742641));
#9543=CARTESIAN_POINT('Ctrl Pts',(-2.77577887489086,5.55729166666709,-3.62317389178086));
#9544=CARTESIAN_POINT('Ctrl Pts',(-3.6342664840072,5.44270833333292,-2.80158903802911));
#9545=CARTESIAN_POINT('Ctrl Pts',(-3.98342954578962,5.38541666666669,-2.30381481802579));
#9546=CARTESIAN_POINT('Ctrl Pts',(-4.46587846537937,5.27083333333332,-1.20726749397333));
#9547=CARTESIAN_POINT('Ctrl Pts',(-4.59893868349712,5.21354166666665,-0.608910969019916));
#9548=CARTESIAN_POINT('Ctrl Pts',(-4.62503287207784,5.09895833333335,0.598504074825539));
#9549=CARTESIAN_POINT('Ctrl Pts',(-4.51801779654147,5.04166666666663,1.20708755469526));
#9550=CARTESIAN_POINT('Ctrl Pts',(-4.07635124961353,4.92708333333338,2.34155232315641));
#9551=CARTESIAN_POINT('Ctrl Pts',(-3.74183771760646,4.86979166666659,2.86697243316876));
#9552=CARTESIAN_POINT('Ctrl Pts',(-2.89278259633321,4.75520833333342,3.75293030985906));
#9553=CARTESIAN_POINT('Ctrl Pts',(-2.37854763406351,4.69791666666658,4.1130920879442));
#9554=CARTESIAN_POINT('Ctrl Pts',(-1.24610867581347,4.58333333333343,4.61040780923455));
#9555=CARTESIAN_POINT('Ctrl Pts',(-0.628335381481812,4.52604166666658,4.74733026287932));
#9556=CARTESIAN_POINT('Ctrl Pts',(0.617928487287482,4.41145833333343,4.77342445149605));
#9557=CARTESIAN_POINT('Ctrl Pts',(1.24592873652376,4.35416666666679,4.66254714036264));
#9558=CARTESIAN_POINT('Ctrl Pts',(2.41628513920584,4.23958333333322,4.20601379180208));
#9559=CARTESIAN_POINT('Ctrl Pts',(2.95816599145146,4.18229166666676,3.86050154342994));
#9560=CARTESIAN_POINT('Ctrl Pts',(3.87159413570613,4.06770833333325,2.98397615463943));
#9561=CARTESIAN_POINT('Ctrl Pts',(4.24275463010319,4.01041666666671,2.45328045009706));
#9562=CARTESIAN_POINT('Ctrl Pts',(4.75493715308532,3.8958333333333,1.28494985765777));
#9563=CARTESIAN_POINT('Ctrl Pts',(4.89572184226387,3.83854166666642,0.647759793932574));
#9564=CARTESIAN_POINT('Ctrl Pts',(4.9218160309119,3.72395833333359,-0.637352899738291));
#9565=CARTESIAN_POINT('Ctrl Pts',(4.80707648417982,3.66666666666662,-1.28476991836542));
#9566=CARTESIAN_POINT('Ctrl Pts',(4.33567633399462,3.55208333333339,-2.49101795524214));
#9567=CARTESIAN_POINT('Ctrl Pts',(3.97916536924807,3.49479166666671,-3.04935954974168));
#9568=CARTESIAN_POINT('Ctrl Pts',(3.075169712951,3.38020833333329,-3.99025796154567));
#9569=CARTESIAN_POINT('Ctrl Pts',(2.52801326612096,3.3229166666668,-4.37241717226731));
#9570=CARTESIAN_POINT('Ctrl Pts',(1.3237910395117,3.20833333333321,-4.89946649693097));
#9571=CARTESIAN_POINT('Ctrl Pts',(0.667184206381905,3.15104166666636,-5.04411342164931));
#9572=CARTESIAN_POINT('Ctrl Pts',(-0.656777312187654,3.03645833333365,-5.07020761032686));
#9573=CARTESIAN_POINT('Ctrl Pts',(-1.32361110020785,2.97916666666654,-4.95160582799841));
#9574=CARTESIAN_POINT('Ctrl Pts',(-2.56575077127763,2.86458333333347,-4.46533887618575));
#9575=CARTESIAN_POINT('Ctrl Pts',(-3.1405531080382,2.80729166666695,-4.09782919506089));
#9576=CARTESIAN_POINT('Ctrl Pts',(-4.10892178737893,2.69270833333305,-3.16636327126786));
#9577=CARTESIAN_POINT('Ctrl Pts',(-4.50207971443576,2.63541666666658,-2.60274608213879));
#9578=CARTESIAN_POINT('Ctrl Pts',(-5.04399584077227,2.52083333333343,-1.36263222137173));
#9579=CARTESIAN_POINT('Ctrl Pts',(-5.1925050010359,2.4635416666663,-0.686608618821642));
#9580=CARTESIAN_POINT('Ctrl Pts',(-5.21859918974068,2.34895833333371,0.67620172462746));
#9581=CARTESIAN_POINT('Ctrl Pts',(-5.09613517181383,2.29166666666676,1.36245228206106));
#9582=CARTESIAN_POINT('Ctrl Pts',(-4.59500141838005,2.17708333333325,2.64048358730238));
#9583=CARTESIAN_POINT('Ctrl Pts',(-4.21649302087059,2.11979166666664,3.23174666634004));
#9584=CARTESIAN_POINT('Ctrl Pts',(-3.25755682958786,2.00520833333337,4.22758561320685));
#9585=CARTESIAN_POINT('Ctrl Pts',(-2.67747889815098,1.94791666666658,4.63174225660692));
#9586=CARTESIAN_POINT('Ctrl Pts',(-1.40147340323737,1.83333333333343,5.18852518461089));
#9587=CARTESIAN_POINT('Ctrl Pts',(-0.706033031254986,1.77604166666627,5.34089658042353));
#9588=CARTESIAN_POINT('Ctrl Pts',(0.695626137060878,1.66145833333374,5.36699076915345));
#9589=CARTESIAN_POINT('Ctrl Pts',(1.40129346391331,1.60416666666663,5.24066451563091));
#9590=CARTESIAN_POINT('Ctrl Pts',(2.71521640332806,1.48958333333338,4.7246639605727));
#9591=CARTESIAN_POINT('Ctrl Pts',(3.32294022464786,1.43229166666683,4.33515684667557));
#9592=CARTESIAN_POINT('Ctrl Pts',(4.34624943902881,1.31770833333318,3.34875038791256));
#9593=CARTESIAN_POINT('Ctrl Pts',(4.76140479878007,1.26041666666641,2.75221171416214));
#9594=CARTESIAN_POINT('Ctrl Pts',(5.3330545284475,1.1458333333336,1.44031458510402));
#9595=CARTESIAN_POINT('Ctrl Pts',(5.48928815981245,1.08854166666688,0.72545744367903));
#9596=CARTESIAN_POINT('Ctrl Pts',(5.51538234856494,0.973958333333134,-0.715050549484959));
#9597=CARTESIAN_POINT('Ctrl Pts',(5.38519385944284,0.916666666666909,-1.44013464577813));
#9598=CARTESIAN_POINT('Ctrl Pts',(4.85432650277048,0.8020833333331,-2.7899492193412));
#9599=CARTESIAN_POINT('Ctrl Pts',(4.4538206724838,0.744791666666392,-3.4141337829535));
#9600=CARTESIAN_POINT('Ctrl Pts',(3.43994394623404,0.630208333333619,-4.46491326485293));
#9601=CARTESIAN_POINT('Ctrl Pts',(2.82694453016243,0.572916666666411,-4.89106734095877));
#9602=CARTESIAN_POINT('Ctrl Pts',(1.47915576698159,0.4583333333336,-5.47758387227856));
#9603=CARTESIAN_POINT('Ctrl Pts',(0.744881856102772,0.401041666666677,-5.63767973920226));
#9604=CARTESIAN_POINT('Ctrl Pts',(-0.73447496190878,0.286458333333334,-5.66377392797554));
#9605=CARTESIAN_POINT('Ctrl Pts',(-1.4789758276525,0.229166666666838,-5.52972320325324));
#9606=CARTESIAN_POINT('Ctrl Pts',(-2.86468203534475,0.114583333333173,-4.9839890449698));
#9607=CARTESIAN_POINT('Ctrl Pts',(-3.50532733285514,0.0572916666665569,
-4.5724845058884));
#9608=CARTESIAN_POINT('Ctrl Pts',(-4.04445221596811,5.20417042793042E-15,
-4.05181100142375));
#9609=CARTESIAN_POINT('Ctrl Pts',(-2.36559314293001,11.,-2.37295192838617));
#9610=CARTESIAN_POINT('Ctrl Pts',(-2.68495589138643,10.9427083333325,-2.0720405595763));
#9611=CARTESIAN_POINT('Ctrl Pts',(-2.94612920879841,10.8854166666664,-1.70595228936294));
#9612=CARTESIAN_POINT('Ctrl Pts',(-3.30964371429254,10.7708333333336,-0.896538039613314));
#9613=CARTESIAN_POINT('Ctrl Pts',(-3.41180604852602,10.7135416666669,-0.453515668913589));
#9614=CARTESIAN_POINT('Ctrl Pts',(-3.4379002366457,10.5989583333331,0.443108774718904));
#9615=CARTESIAN_POINT('Ctrl Pts',(-3.36178304590245,10.5416666666666,0.896358100460257));
#9616=CARTESIAN_POINT('Ctrl Pts',(-3.03905091217473,10.4270833333334,1.74368979436799));
#9617=CARTESIAN_POINT('Ctrl Pts',(-2.79252711081109,10.3697916666664,2.13742396723561));
#9618=CARTESIAN_POINT('Ctrl Pts',(-2.16323413009096,10.2552083333337,2.80361970275416));
#9619=CARTESIAN_POINT('Ctrl Pts',(-1.78068510549046,10.1979166666664,3.07579175088966));
#9620=CARTESIAN_POINT('Ctrl Pts',(-0.935379221363662,10.0833333333336,3.45417305821104));
#9621=CARTESIAN_POINT('Ctrl Pts',(-0.472940081479242,10.0260416666666,3.56019762788479));
#9622=CARTESIAN_POINT('Ctrl Pts',(0.462533187284589,9.91145833333345,3.58629181608734));
#9623=CARTESIAN_POINT('Ctrl Pts',(0.935199282188079,9.85416666666669,3.50631238974053));
#9624=CARTESIAN_POINT('Ctrl Pts',(1.81842261051809,9.73958333333332,3.16871345434639));
#9625=CARTESIAN_POINT('Ctrl Pts',(2.22861752543397,9.68229166666673,2.91119093668731));
#9626=CARTESIAN_POINT('Ctrl Pts',(2.92228352868554,9.56770833333328,2.25442768834444));
#9627=CARTESIAN_POINT('Ctrl Pts',(3.20545429299277,9.51041666666666,1.85541792160244));
#9628=CARTESIAN_POINT('Ctrl Pts',(3.59870240211769,9.39583333333334,0.974220403129539));
#9629=CARTESIAN_POINT('Ctrl Pts',(3.70858920724845,9.3385416666664,0.492364494026195));
#9630=CARTESIAN_POINT('Ctrl Pts',(3.73468339552408,9.22395833333361,-0.481957599831572));
#9631=CARTESIAN_POINT('Ctrl Pts',(3.65084173357628,9.16666666666689,-0.974040463933888));
#9632=CARTESIAN_POINT('Ctrl Pts',(3.29837599652037,9.05208333333312,-1.8931554266502));
#9633=CARTESIAN_POINT('Ctrl Pts',(3.02985476255422,8.99479166666641,-2.31981108364774));
#9634=CARTESIAN_POINT('Ctrl Pts',(2.34562124660724,8.8802083333336,-3.04094735460153));
#9635=CARTESIAN_POINT('Ctrl Pts',(1.93015073770027,8.82291666666647,-3.33511683510577));
#9636=CARTESIAN_POINT('Ctrl Pts',(1.01306158490958,8.70833333333354,-3.74323174601444));
#9637=CARTESIAN_POINT('Ctrl Pts',(0.511788906557484,8.6510416666665,-3.85698078661577));
#9638=CARTESIAN_POINT('Ctrl Pts',(-0.501382012362897,8.53645833333351,-3.88307497495716));
#9639=CARTESIAN_POINT('Ctrl Pts',(-1.01288164569554,8.47916666666683,-3.79537107740945));
#9640=CARTESIAN_POINT('Ctrl Pts',(-1.96788824276646,8.36458333333318,-3.42803853869692));
#9641=CARTESIAN_POINT('Ctrl Pts',(-2.41100464187403,8.30729166666683,-3.14851858841386));
#9642=CARTESIAN_POINT('Ctrl Pts',(-3.159611180505,8.1927083333332,-2.43681480487731));
#9643=CARTESIAN_POINT('Ctrl Pts',(-3.46477937722837,8.13541666666656,-2.00488355378617));
#9644=CARTESIAN_POINT('Ctrl Pts',(-3.8877610899016,8.02083333333345,-1.05190276670153));
#9645=CARTESIAN_POINT('Ctrl Pts',(-4.00537236598643,7.96354166666637,-0.531213319073915));
#9646=CARTESIAN_POINT('Ctrl Pts',(-4.03146655438691,7.84895833333365,0.520806424879362));
#9647=CARTESIAN_POINT('Ctrl Pts',(-3.93990042124014,7.79166666666665,1.05172282747159));
#9648=CARTESIAN_POINT('Ctrl Pts',(-3.55770108087595,7.67708333333337,2.04262105886835));
#9649=CARTESIAN_POINT('Ctrl Pts',(-3.26718241426475,7.61979166666659,2.50219820011361));
#9650=CARTESIAN_POINT('Ctrl Pts',(-2.52800836315612,7.50520833333343,3.27827500639517));
#9651=CARTESIAN_POINT('Ctrl Pts',(-2.07961636986072,7.44791666666668,3.59444191935829));
#9652=CARTESIAN_POINT('Ctrl Pts',(-1.09074394850484,7.33333333333333,4.03229043378143));
#9653=CARTESIAN_POINT('Ctrl Pts',(-0.550637731576509,7.27604166666629,4.15376394536062));
#9654=CARTESIAN_POINT('Ctrl Pts',(0.540230837381994,7.16145833333372,4.17985813381312));
#9655=CARTESIAN_POINT('Ctrl Pts',(1.09056400926098,7.10416666666678,4.08442976506864));
#9656=CARTESIAN_POINT('Ctrl Pts',(2.11735387495688,6.98958333333323,3.68736362305719));
#9657=CARTESIAN_POINT('Ctrl Pts',(2.59339175836345,6.93229166666724,3.38584624010982));
#9658=CARTESIAN_POINT('Ctrl Pts',(3.3969388322751,6.81770833333277,2.61920192144075));
#9659=CARTESIAN_POINT('Ctrl Pts',(3.72410446149635,6.76041666666712,2.15434918592434));
#9660=CARTESIAN_POINT('Ctrl Pts',(4.17681977765313,6.64583333333289,1.12958513031907));
#9661=CARTESIAN_POINT('Ctrl Pts',(4.30215552473732,6.58854166666688,0.570062144068889));
#9662=CARTESIAN_POINT('Ctrl Pts',(4.32824971323683,6.47395833333313,-0.559655249874413));
#9663=CARTESIAN_POINT('Ctrl Pts',(4.22895910889563,6.41666666666645,-1.12940519106012));
#9664=CARTESIAN_POINT('Ctrl Pts',(3.81702616523991,6.30208333333356,-2.19208669103568));
#9665=CARTESIAN_POINT('Ctrl Pts',(3.50451006594675,6.24479166666656,-2.68458531662391));
#9666=CARTESIAN_POINT('Ctrl Pts',(2.71039547973352,6.13020833333345,-3.51560265814439));
#9667=CARTESIAN_POINT('Ctrl Pts',(2.22908200197935,6.07291666666717,-3.85376700363998));
#9668=CARTESIAN_POINT('Ctrl Pts',(1.16842631214193,5.95833333333284,-4.32134912151925));
#9669=CARTESIAN_POINT('Ctrl Pts',(0.589486556547344,5.90104166666655,-4.45054710411593));
#9670=CARTESIAN_POINT('Ctrl Pts',(-0.579079662352908,5.78645833333346,-4.47664129265863));
#9671=CARTESIAN_POINT('Ctrl Pts',(-1.16824637287424,5.72916666666705,-4.37348845271886));
#9672=CARTESIAN_POINT('Ctrl Pts',(-2.26681950709949,5.61458333333296,-3.94668870742641));
#9673=CARTESIAN_POINT('Ctrl Pts',(-2.77577887489086,5.55729166666709,-3.62317389178086));
#9674=CARTESIAN_POINT('Ctrl Pts',(-3.6342664840072,5.44270833333292,-2.80158903802911));
#9675=CARTESIAN_POINT('Ctrl Pts',(-3.98342954578962,5.38541666666669,-2.30381481802579));
#9676=CARTESIAN_POINT('Ctrl Pts',(-4.46587846537937,5.27083333333332,-1.20726749397333));
#9677=CARTESIAN_POINT('Ctrl Pts',(-4.59893868349712,5.21354166666665,-0.608910969019916));
#9678=CARTESIAN_POINT('Ctrl Pts',(-4.62503287207784,5.09895833333335,0.598504074825539));
#9679=CARTESIAN_POINT('Ctrl Pts',(-4.51801779654147,5.04166666666663,1.20708755469526));
#9680=CARTESIAN_POINT('Ctrl Pts',(-4.07635124961353,4.92708333333338,2.34155232315641));
#9681=CARTESIAN_POINT('Ctrl Pts',(-3.74183771760646,4.86979166666659,2.86697243316876));
#9682=CARTESIAN_POINT('Ctrl Pts',(-2.89278259633321,4.75520833333342,3.75293030985906));
#9683=CARTESIAN_POINT('Ctrl Pts',(-2.37854763406351,4.69791666666658,4.1130920879442));
#9684=CARTESIAN_POINT('Ctrl Pts',(-1.24610867581347,4.58333333333343,4.61040780923455));
#9685=CARTESIAN_POINT('Ctrl Pts',(-0.628335381481812,4.52604166666658,4.74733026287932));
#9686=CARTESIAN_POINT('Ctrl Pts',(0.617928487287482,4.41145833333343,4.77342445149605));
#9687=CARTESIAN_POINT('Ctrl Pts',(1.24592873652376,4.35416666666679,4.66254714036264));
#9688=CARTESIAN_POINT('Ctrl Pts',(2.41628513920584,4.23958333333322,4.20601379180208));
#9689=CARTESIAN_POINT('Ctrl Pts',(2.95816599145146,4.18229166666676,3.86050154342994));
#9690=CARTESIAN_POINT('Ctrl Pts',(3.87159413570613,4.06770833333325,2.98397615463943));
#9691=CARTESIAN_POINT('Ctrl Pts',(4.24275463010319,4.01041666666671,2.45328045009706));
#9692=CARTESIAN_POINT('Ctrl Pts',(4.75493715308532,3.8958333333333,1.28494985765777));
#9693=CARTESIAN_POINT('Ctrl Pts',(4.89572184226387,3.83854166666642,0.647759793932574));
#9694=CARTESIAN_POINT('Ctrl Pts',(4.9218160309119,3.72395833333359,-0.637352899738291));
#9695=CARTESIAN_POINT('Ctrl Pts',(4.80707648417982,3.66666666666662,-1.28476991836542));
#9696=CARTESIAN_POINT('Ctrl Pts',(4.33567633399462,3.55208333333339,-2.49101795524214));
#9697=CARTESIAN_POINT('Ctrl Pts',(3.97916536924807,3.49479166666671,-3.04935954974168));
#9698=CARTESIAN_POINT('Ctrl Pts',(3.075169712951,3.38020833333329,-3.99025796154567));
#9699=CARTESIAN_POINT('Ctrl Pts',(2.52801326612096,3.3229166666668,-4.37241717226731));
#9700=CARTESIAN_POINT('Ctrl Pts',(1.3237910395117,3.20833333333321,-4.89946649693097));
#9701=CARTESIAN_POINT('Ctrl Pts',(0.667184206381905,3.15104166666636,-5.04411342164931));
#9702=CARTESIAN_POINT('Ctrl Pts',(-0.656777312187654,3.03645833333365,-5.07020761032686));
#9703=CARTESIAN_POINT('Ctrl Pts',(-1.32361110020785,2.97916666666654,-4.95160582799841));
#9704=CARTESIAN_POINT('Ctrl Pts',(-2.56575077127763,2.86458333333347,-4.46533887618575));
#9705=CARTESIAN_POINT('Ctrl Pts',(-3.1405531080382,2.80729166666695,-4.09782919506089));
#9706=CARTESIAN_POINT('Ctrl Pts',(-4.10892178737893,2.69270833333305,-3.16636327126786));
#9707=CARTESIAN_POINT('Ctrl Pts',(-4.50207971443576,2.63541666666658,-2.60274608213879));
#9708=CARTESIAN_POINT('Ctrl Pts',(-5.04399584077227,2.52083333333343,-1.36263222137173));
#9709=CARTESIAN_POINT('Ctrl Pts',(-5.1925050010359,2.4635416666663,-0.686608618821642));
#9710=CARTESIAN_POINT('Ctrl Pts',(-5.21859918974068,2.34895833333371,0.67620172462746));
#9711=CARTESIAN_POINT('Ctrl Pts',(-5.09613517181383,2.29166666666676,1.36245228206106));
#9712=CARTESIAN_POINT('Ctrl Pts',(-4.59500141838005,2.17708333333325,2.64048358730238));
#9713=CARTESIAN_POINT('Ctrl Pts',(-4.21649302087059,2.11979166666664,3.23174666634004));
#9714=CARTESIAN_POINT('Ctrl Pts',(-3.25755682958786,2.00520833333337,4.22758561320685));
#9715=CARTESIAN_POINT('Ctrl Pts',(-2.67747889815098,1.94791666666658,4.63174225660692));
#9716=CARTESIAN_POINT('Ctrl Pts',(-1.40147340323737,1.83333333333343,5.18852518461089));
#9717=CARTESIAN_POINT('Ctrl Pts',(-0.706033031254986,1.77604166666627,5.34089658042353));
#9718=CARTESIAN_POINT('Ctrl Pts',(0.695626137060878,1.66145833333374,5.36699076915345));
#9719=CARTESIAN_POINT('Ctrl Pts',(1.40129346391331,1.60416666666663,5.24066451563091));
#9720=CARTESIAN_POINT('Ctrl Pts',(2.71521640332806,1.48958333333338,4.7246639605727));
#9721=CARTESIAN_POINT('Ctrl Pts',(3.32294022464786,1.43229166666683,4.33515684667557));
#9722=CARTESIAN_POINT('Ctrl Pts',(4.34624943902881,1.31770833333318,3.34875038791256));
#9723=CARTESIAN_POINT('Ctrl Pts',(4.76140479878007,1.26041666666641,2.75221171416214));
#9724=CARTESIAN_POINT('Ctrl Pts',(5.3330545284475,1.1458333333336,1.44031458510402));
#9725=CARTESIAN_POINT('Ctrl Pts',(5.48928815981245,1.08854166666688,0.72545744367903));
#9726=CARTESIAN_POINT('Ctrl Pts',(5.51538234856494,0.973958333333134,-0.715050549484959));
#9727=CARTESIAN_POINT('Ctrl Pts',(5.38519385944284,0.916666666666909,-1.44013464577813));
#9728=CARTESIAN_POINT('Ctrl Pts',(4.85432650277048,0.8020833333331,-2.7899492193412));
#9729=CARTESIAN_POINT('Ctrl Pts',(4.4538206724838,0.744791666666392,-3.4141337829535));
#9730=CARTESIAN_POINT('Ctrl Pts',(3.43994394623404,0.630208333333619,-4.46491326485293));
#9731=CARTESIAN_POINT('Ctrl Pts',(2.82694453016243,0.572916666666411,-4.89106734095877));
#9732=CARTESIAN_POINT('Ctrl Pts',(1.47915576698159,0.4583333333336,-5.47758387227856));
#9733=CARTESIAN_POINT('Ctrl Pts',(0.744881856102772,0.401041666666677,-5.63767973920226));
#9734=CARTESIAN_POINT('Ctrl Pts',(-0.73447496190878,0.286458333333334,-5.66377392797554));
#9735=CARTESIAN_POINT('Ctrl Pts',(-1.4789758276525,0.229166666666838,-5.52972320325324));
#9736=CARTESIAN_POINT('Ctrl Pts',(-2.86468203534475,0.114583333333173,-4.9839890449698));
#9737=CARTESIAN_POINT('Ctrl Pts',(-3.50532733285514,0.0572916666665569,
-4.5724845058884));
#9738=CARTESIAN_POINT('Ctrl Pts',(-4.04445221596811,5.20417042793042E-15,
-4.05181100142375));
#9739=CARTESIAN_POINT('Ctrl Pts',(-2.40035683308082,11.3467255152722,-2.34019673175572));
#9740=CARTESIAN_POINT('Ctrl Pts',(-2.71543193620083,11.2894338486048,-2.03473480641482));
#9741=CARTESIAN_POINT('Ctrl Pts',(-2.97141448964516,11.2321421819387,-1.66495030044034));
#9742=CARTESIAN_POINT('Ctrl Pts',(-3.32352361490692,11.1175588486058,-0.850409340498224));
#9743=CARTESIAN_POINT('Ctrl Pts',(-3.4194758201212,11.0602671819391,-0.405958512493029));
#9744=CARTESIAN_POINT('Ctrl Pts',(-3.43307090382695,10.9456838486053,0.491037743700738));
#9745=CARTESIAN_POINT('Ctrl Pts',(-3.35066965504748,10.8883921819389,0.943230278421825));
#9746=CARTESIAN_POINT('Ctrl Pts',(-3.01624756806638,10.7738088486056,1.78612228216488));
#9747=CARTESIAN_POINT('Ctrl Pts',(-2.76432247051982,10.7165171819386,2.17647530254211));
#9748=CARTESIAN_POINT('Ctrl Pts',(-2.12592837712132,10.6019338486059,2.83409574774927));
#9749=CARTESIAN_POINT('Ctrl Pts',(-1.7396831165707,10.5446421819387,3.10107703174287));
#9750=CARTESIAN_POINT('Ctrl Pts',(-0.889250522245734,10.4300588486058,3.46805295881896));
#9751=CARTESIAN_POINT('Ctrl Pts',(-0.425382925058827,10.3727671819388,3.56786739948684));
#9752=CARTESIAN_POINT('Ctrl Pts',(0.510462156266568,10.2581838486057,3.58146248326171));
#9753=CARTESIAN_POINT('Ctrl Pts',(0.982071460151994,10.2008921819389,3.49519899889172));
#9754=CARTESIAN_POINT('Ctrl Pts',(1.86085509831263,10.0863088486056,3.14591011023186));
#9755=CARTESIAN_POINT('Ctrl Pts',(2.26766886074488,10.029017181939,2.88298629640079));
#9756=CARTESIAN_POINT('Ctrl Pts',(2.95275957367625,9.91443384860552,2.21712193537007));
#9757=CARTESIAN_POINT('Ctrl Pts',(3.2307395738517,9.8571421819389,1.81441593268519));
#9758=CARTESIAN_POINT('Ctrl Pts',(3.61258230271989,9.74255884860558,0.9280917040091));
#9759=CARTESIAN_POINT('Ctrl Pts',(3.71625897885657,9.68526718193864,0.444807337606009));
#9760=CARTESIAN_POINT('Ctrl Pts',(3.72985406269238,9.57068384860584,-0.52988656881378));
#9761=CARTESIAN_POINT('Ctrl Pts',(3.63972834273301,9.51339218193913,-1.02091264189992));
#9762=CARTESIAN_POINT('Ctrl Pts',(3.2755726524003,9.39880884860535,-1.93558791444263));
#9763=CARTESIAN_POINT('Ctrl Pts',(3.00165012227183,9.34151718193865,-2.35886241896257));
#9764=CARTESIAN_POINT('Ctrl Pts',(2.30831549362873,9.22693384860583,-3.07142339958832));
#9765=CARTESIAN_POINT('Ctrl Pts',(1.88914874878537,9.1696421819387,-3.3604021159697));
#9766=CARTESIAN_POINT('Ctrl Pts',(0.966932885786784,9.05505884860578,-3.75711164661164));
#9767=CARTESIAN_POINT('Ctrl Pts',(0.46423175013744,8.99776718193874,-3.86465055822944));
#9768=CARTESIAN_POINT('Ctrl Pts',(-0.549310981345247,8.88318384860575,-3.87824564211992));
#9769=CARTESIAN_POINT('Ctrl Pts',(-1.05975382366345,8.82589218193907,-3.78425768657106));
#9770=CARTESIAN_POINT('Ctrl Pts',(-2.01032073055702,8.71130884860541,-3.40523519457197));
#9771=CARTESIAN_POINT('Ctrl Pts',(-2.45005597719243,8.65401718193906,-3.12031394813519));
#9772=CARTESIAN_POINT('Ctrl Pts',(-3.19008722548821,8.53943384860543,-2.39950905189507));
#9773=CARTESIAN_POINT('Ctrl Pts',(-3.49006465809683,8.48214218193879,-1.96388156487328));
#9774=CARTESIAN_POINT('Ctrl Pts',(-3.90164099049427,8.36755884860569,-1.00577406757672));
#9775=CARTESIAN_POINT('Ctrl Pts',(-4.01304213760465,8.3102671819386,-0.483656162654029));
#9776=CARTESIAN_POINT('Ctrl Pts',(-4.02663722154512,8.19568384860588,0.568735393861871));
#9777=CARTESIAN_POINT('Ctrl Pts',(-3.92878703040616,8.13839218193865,1.09859500544122));
#9778=CARTESIAN_POINT('Ctrl Pts',(-3.5348977367466,8.02380884860583,2.08505354665718));
#9779=CARTESIAN_POINT('Ctrl Pts',(-3.23897777398945,7.96651718193906,2.54124953543508));
#9780=CARTESIAN_POINT('Ctrl Pts',(-2.49070261017052,7.85193384860543,3.30875105137532));
#9781=CARTESIAN_POINT('Ctrl Pts',(-2.03861438094966,7.79464218193892,3.61972720023077));
#9782=CARTESIAN_POINT('Ctrl Pts',(-1.0446152493782,7.68005884860556,4.04617033437007));
#9783=CARTESIAN_POINT('Ctrl Pts',(-0.503080575156725,7.62276718193853,4.16143371698328));
#9784=CARTESIAN_POINT('Ctrl Pts',(0.588159806364604,7.50818384860596,4.17502880096689));
#9785=CARTESIAN_POINT('Ctrl Pts',(1.13743618723204,7.45089218193902,4.07331637423875));
#9786=CARTESIAN_POINT('Ctrl Pts',(2.15978636274428,7.33630884860546,3.66456027892374));
#9787=CARTESIAN_POINT('Ctrl Pts',(2.63244309368768,7.27901718193947,3.35764159983753));
#9788=CARTESIAN_POINT('Ctrl Pts',(3.42741487725249,7.16443384860501,2.58189616845213));
#9789=CARTESIAN_POINT('Ctrl Pts',(3.74938974237272,7.10714218193936,2.11334719701498));
#9790=CARTESIAN_POINT('Ctrl Pts',(4.19069967823789,6.99255884860513,1.08345643119075));
#9791=CARTESIAN_POINT('Ctrl Pts',(4.30982529636403,6.93526718193912,0.522504987649244));
#9792=CARTESIAN_POINT('Ctrl Pts',(4.32342038038655,6.82068384860537,-0.607584218857162));
#9793=CARTESIAN_POINT('Ctrl Pts',(4.21784571806929,6.76339218193869,-1.17627736903264));
#9794=CARTESIAN_POINT('Ctrl Pts',(3.79422282110293,6.6488088486058,-2.23451917882162));
#9795=CARTESIAN_POINT('Ctrl Pts',(3.47630542567715,6.5915171819388,-2.72363665195073));
#9796=CARTESIAN_POINT('Ctrl Pts',(2.67308972674222,6.47693384860569,-3.54607870311919));
#9797=CARTESIAN_POINT('Ctrl Pts',(2.18808001307138,6.41964218193941,-3.87905228451955));
#9798=CARTESIAN_POINT('Ctrl Pts',(1.1222976130122,6.30505884860508,-4.33522902210081));
#9799=CARTESIAN_POINT('Ctrl Pts',(0.541929400127819,6.24776718193879,-4.45821687574607));
#9800=CARTESIAN_POINT('Ctrl Pts',(-0.627008631335778,6.1331838486057,-4.47181195980492));
#9801=CARTESIAN_POINT('Ctrl Pts',(-1.21511855084784,6.07589218193929,-4.3623750618956));
#9802=CARTESIAN_POINT('Ctrl Pts',(-2.30925199488436,5.9613088486052,-3.92388536328634));
#9803=CARTESIAN_POINT('Ctrl Pts',(-2.81483021022013,5.90401718193932,-3.59496925151373));
#9804=CARTESIAN_POINT('Ctrl Pts',(-3.66474252897955,5.78943384860516,-2.76428328503534));
#9805=CARTESIAN_POINT('Ctrl Pts',(-4.0087148266721,5.73214218193892,-2.26281282911923));
#9806=CARTESIAN_POINT('Ctrl Pts',(-4.47975836595802,5.61755884860556,-1.1611387948422));
#9807=CARTESIAN_POINT('Ctrl Pts',(-4.60660845513052,5.56026718193889,-0.561353812600464));
#9808=CARTESIAN_POINT('Ctrl Pts',(-4.62020353922087,5.44568384860559,0.646433043808482));
#9809=CARTESIAN_POINT('Ctrl Pts',(-4.50690440572112,5.38839218193887,1.25395973267003));
#9810=CARTESIAN_POINT('Ctrl Pts',(-4.05354790547054,5.27380884860562,2.38398481094011));
#9811=CARTESIAN_POINT('Ctrl Pts',(-3.71363307734148,5.21651718193883,2.90602376850005));
#9812=CARTESIAN_POINT('Ctrl Pts',(-2.85547684333729,5.10193384860566,3.78340635482939));
#9813=CARTESIAN_POINT('Ctrl Pts',(-2.33754564515818,5.04464218193881,4.13837736882935));
#9814=CARTESIAN_POINT('Ctrl Pts',(-1.1999799766811,4.93005884860567,4.62428770981052));
#9815=CARTESIAN_POINT('Ctrl Pts',(-0.580778225062417,4.87276718193882,4.75500003451575));
#9816=CARTESIAN_POINT('Ctrl Pts',(0.665857456270481,4.75818384860566,4.76859511863605));
#9817=CARTESIAN_POINT('Ctrl Pts',(1.2928009144995,4.70089218193903,4.65143374954513));
#9818=CARTESIAN_POINT('Ctrl Pts',(2.45871762698856,4.58630884860546,4.18321044765625));
#9819=CARTESIAN_POINT('Ctrl Pts',(2.99721732678471,4.529017181939,3.83229690316695));
#9820=CARTESIAN_POINT('Ctrl Pts',(3.9020701806745,4.41443384860549,2.94667040164152));
#9821=CARTESIAN_POINT('Ctrl Pts',(4.2680399109909,4.35714218193895,2.41227846119283));
#9822=CARTESIAN_POINT('Ctrl Pts',(4.76881705365873,4.24255884860554,1.2388211585243));
#9823=CARTESIAN_POINT('Ctrl Pts',(4.90339161390277,4.18526718193866,0.600202637513305));
#9824=CARTESIAN_POINT('Ctrl Pts',(4.91698669804943,4.07068384860583,-0.685281868721417));
#9825=CARTESIAN_POINT('Ctrl Pts',(4.79596309336461,4.01339218193886,-1.33164209634213));
#9826=CARTESIAN_POINT('Ctrl Pts',(4.31287298984649,3.89880884860562,-2.53345044302389));
#9827=CARTESIAN_POINT('Ctrl Pts',(3.95096072898711,3.84151718193895,-3.08841088507667));
#9828=CARTESIAN_POINT('Ctrl Pts',(3.03786395995105,3.72693384860553,-4.02073400651229));
#9829=CARTESIAN_POINT('Ctrl Pts',(2.48701127721779,3.66964218193904,-4.39770245315732));
#9830=CARTESIAN_POINT('Ctrl Pts',(1.27766234037718,3.55505884860545,-4.91334639750207));
#9831=CARTESIAN_POINT('Ctrl Pts',(0.619627049962736,3.4977671819386,-5.05178319329073));
#9832=CARTESIAN_POINT('Ctrl Pts',(-0.704706281170879,3.38318384860588,-5.06537827746187));
#9833=CARTESIAN_POINT('Ctrl Pts',(-1.37048327818541,3.32589218193878,-4.94049243718524));
#9834=CARTESIAN_POINT('Ctrl Pts',(-2.60818325905853,3.21130884860571,-4.44253553203559));
#9835=CARTESIAN_POINT('Ctrl Pts',(-3.17960444337468,3.15401718193919,-4.06962455480154));
#9836=CARTESIAN_POINT('Ctrl Pts',(-4.13939783234407,3.03943384860528,-3.1290575182663));
#9837=CARTESIAN_POINT('Ctrl Pts',(-4.52736499532796,2.98214218193882,-2.5617440932366));
#9838=CARTESIAN_POINT('Ctrl Pts',(-5.05787574134119,2.86755884860567,-1.31650352223623));
#9839=CARTESIAN_POINT('Ctrl Pts',(-5.20017477267972,2.81026718193854,-0.639051462402516));
#9840=CARTESIAN_POINT('Ctrl Pts',(-5.21376985687329,2.69568384860595,0.724130693610728));
#9841=CARTESIAN_POINT('Ctrl Pts',(-5.08502178100269,2.638392181939,1.40932446003936));
#9842=CARTESIAN_POINT('Ctrl Pts',(-4.57219807422785,2.52380884860549,2.68291607508254));
#9843=CARTESIAN_POINT('Ctrl Pts',(-4.18828838061282,2.46651718193888,3.27079800167798));
#9844=CARTESIAN_POINT('Ctrl Pts',(-3.22025107658473,2.3519338486056,4.25806165817053));
#9845=CARTESIAN_POINT('Ctrl Pts',(-2.63647690924959,2.29464218193882,4.65702753750094));
#9846=CARTESIAN_POINT('Ctrl Pts',(-1.35534470410106,2.18005884860566,5.20240508517798));
#9847=CARTESIAN_POINT('Ctrl Pts',(-0.658475874835927,2.12276718193851,5.34856635206931));
#9848=CARTESIAN_POINT('Ctrl Pts',(0.743555106044213,2.00818384860598,5.3621614362841));
#9849=CARTESIAN_POINT('Ctrl Pts',(1.44816564189249,1.95089218193886,5.22955112482197));
#9850=CARTESIAN_POINT('Ctrl Pts',(2.75764889110733,1.83630884860562,4.70186061641829));
#9851=CARTESIAN_POINT('Ctrl Pts',(3.36199155998716,1.77901718193906,4.30695220641913));
#9852=CARTESIAN_POINT('Ctrl Pts',(4.37672548399112,1.66443384860542,3.3114446349081));
#9853=CARTESIAN_POINT('Ctrl Pts',(4.78669007967579,1.60714218193865,2.71120972526174));
#9854=CARTESIAN_POINT('Ctrl Pts',(5.3469344290129,1.49255884860583,1.39418588596674));
#9855=CARTESIAN_POINT('Ctrl Pts',(5.49695793145999,1.43526718193912,0.677900287260056));
#9856=CARTESIAN_POINT('Ctrl Pts',(5.51055301569383,1.32068384860537,-0.76297951846838));
#9857=CARTESIAN_POINT('Ctrl Pts',(5.37408046863567,1.26339218193915,-1.4870068237579));
#9858=CARTESIAN_POINT('Ctrl Pts',(4.83152315861431,1.14880884860534,-2.83238170711989));
#9859=CARTESIAN_POINT('Ctrl Pts',(4.42561603222875,1.09151718193863,-3.45318511829405));
#9860=CARTESIAN_POINT('Ctrl Pts',(3.40263819322818,0.976933848605856,-4.49538930981399));
#9861=CARTESIAN_POINT('Ctrl Pts',(2.78594254126256,0.919642181938648,-4.91635262185619));
#9862=CARTESIAN_POINT('Ctrl Pts',(1.43302706784377,0.805058848605838,-5.49146377284226));
#9863=CARTESIAN_POINT('Ctrl Pts',(0.697324699683797,0.747767181938915,-5.64534951085169));
#9864=CARTESIAN_POINT('Ctrl Pts',(-0.782403930892199,0.633183848605571,
-5.65894459510253));
#9865=CARTESIAN_POINT('Ctrl Pts',(-1.5258480056327,0.575892181939075,-5.51860981244762));
#9866=CARTESIAN_POINT('Ctrl Pts',(-2.90711452312302,0.46130884860541,-4.96118570081208));
#9867=CARTESIAN_POINT('Ctrl Pts',(-3.54437866826175,0.404017181938794,-4.5442798657039));
#9868=CARTESIAN_POINT('Ctrl Pts',(-4.07921590611891,0.346725515272242,-4.0190558047933));
#9869=CARTESIAN_POINT('Ctrl Pts',(-2.16033767231584,11.3467255152722,-2.08546000007833));
#9870=CARTESIAN_POINT('Ctrl Pts',(-2.44206781427164,11.2894338486048,-1.81141651031886));
#9871=CARTESIAN_POINT('Ctrl Pts',(-2.67096558433259,11.2321421819387,-1.47966819216879));
#9872=CARTESIAN_POINT('Ctrl Pts',(-2.98550788648136,11.1175588486058,-0.748702056168519));
#9873=CARTESIAN_POINT('Ctrl Pts',(-3.07099283278885,11.0602671819391,-0.349756983242139));
#9874=CARTESIAN_POINT('Ctrl Pts',(-3.0818633980033,10.9456838486053,0.455650002839366));
#9875=CARTESIAN_POINT('Ctrl Pts',(-3.00720596150024,10.8883921819389,0.861795055291616));
#9876=CARTESIAN_POINT('Ctrl Pts',(-2.70531644391264,10.7738088486056,1.61902697886803));
#9877=CARTESIAN_POINT('Ctrl Pts',(-2.47816730458498,10.7165171819386,1.96980110153648));
#9878=CARTESIAN_POINT('Ctrl Pts',(-1.90261007970139,10.6019338486059,2.56073162722495));
#9879=CARTESIAN_POINT('Ctrl Pts',(-1.55440100825198,10.5446421819387,2.80062812645173));
#9880=CARTESIAN_POINT('Ctrl Pts',(-0.787543237963199,10.4300588486058,3.13003723037197));
#9881=CARTESIAN_POINT('Ctrl Pts',(-0.369181395757753,10.3727671819388,3.21938441215601));
#9882=CARTESIAN_POINT('Ctrl Pts',(0.475074415355009,10.2581838486057,3.23025497743655));
#9883=CARTESIAN_POINT('Ctrl Pts',(0.900636237067393,10.2008921819389,3.15173530532716));
#9884=CARTESIAN_POINT('Ctrl Pts',(1.69375979497017,10.0863088486056,2.83497898609545));
#9885=CARTESIAN_POINT('Ctrl Pts',(2.0609946597737,10.029017181939,2.59683113043342));
#9886=CARTESIAN_POINT('Ctrl Pts',(2.67939545311748,9.91443384860552,1.99380363798266));
#9887=CARTESIAN_POINT('Ctrl Pts',(2.93029066857928,9.8571421819389,1.62913382432459));
#9888=CARTESIAN_POINT('Ctrl Pts',(3.27456657425417,9.74255884860558,0.826384419768452));
#9889=CARTESIAN_POINT('Ctrl Pts',(3.36777599152708,9.68526718193864,0.388605808260406));
#9890=CARTESIAN_POINT('Ctrl Pts',(3.37864655686589,9.57068384860584,-0.49449882785769));
#9891=CARTESIAN_POINT('Ctrl Pts',(3.29626464915295,9.51339218193913,-0.939477418855915));
#9892=CARTESIAN_POINT('Ctrl Pts',(2.96464152827939,9.39880884860535,-1.76849261105957));
#9893=CARTESIAN_POINT('Ctrl Pts',(2.71549495627589,9.34151718193865,-2.15218821802195));
#9894=CARTESIAN_POINT('Ctrl Pts',(2.0849971962699,9.22693384860583,-2.79805927899898));
#9895=CARTESIAN_POINT('Ctrl Pts',(1.70386664038741,9.1696421819387,-3.05995321071421));
#9896=CARTESIAN_POINT('Ctrl Pts',(0.865225601583496,9.05505884860578,-3.419095918129));
#9897=CARTESIAN_POINT('Ctrl Pts',(0.408030220752219,8.99776718193874,-3.51616757090102));
#9898=CARTESIAN_POINT('Ctrl Pts',(-0.513923240349536,8.88318384860575,-3.52703813629236));
#9899=CARTESIAN_POINT('Ctrl Pts',(-0.978318600655415,8.82589218193907,-3.44079399297743));
#9900=CARTESIAN_POINT('Ctrl Pts',(-1.84322542713799,8.71130884860541,-3.09430407046464));
#9901=CARTESIAN_POINT('Ctrl Pts',(-2.24338177627905,8.65401718193906,-2.8341587821133));
#9902=CARTESIAN_POINT('Ctrl Pts',(-2.91672310487163,8.53943384860543,-2.1761907545622));
#9903=CARTESIAN_POINT('Ctrl Pts',(-3.18961575285625,8.48214218193879,-1.77859945644224));
#9904=CARTESIAN_POINT('Ctrl Pts',(-3.56362526199671,8.36755884860569,-0.904066783406526));
#9905=CARTESIAN_POINT('Ctrl Pts',(-3.66455915027763,8.3102671819386,-0.427454633233268));
#9906=CARTESIAN_POINT('Ctrl Pts',(-3.67542971571615,8.19568384860588,0.533347652830617));
#9907=CARTESIAN_POINT('Ctrl Pts',(-3.58532333680026,8.13839218193865,1.01715978246527));
#9908=CARTESIAN_POINT('Ctrl Pts',(-3.22396661265153,8.02380884860583,1.91795824320607));
#9909=CARTESIAN_POINT('Ctrl Pts',(-2.95282260794454,7.96651718193906,2.33457533454633));
#9910=CARTESIAN_POINT('Ctrl Pts',(-2.26738431286067,7.85193384860543,3.03538693073411));
#9911=CARTESIAN_POINT('Ctrl Pts',(-1.85333227248862,7.79464218193892,3.31927829500387));
#9912=CARTESIAN_POINT('Ctrl Pts',(-0.942907965238003,7.68005884860556,3.70815460585884));
#9913=CARTESIAN_POINT('Ctrl Pts',(-0.446879045704217,7.62276718193853,3.81295072965703));
#9914=CARTESIAN_POINT('Ctrl Pts',(0.552772065301601,7.50818384860596,3.82382129513715));
#9915=CARTESIAN_POINT('Ctrl Pts',(1.05600096428514,7.45089218193902,3.7298526806217));
#9916=CARTESIAN_POINT('Ctrl Pts',(1.99269105926411,7.33630884860546,3.35362915483982));
#9917=CARTESIAN_POINT('Ctrl Pts',(2.42576889282071,7.27901718193947,3.07148643377194));
#9918=CARTESIAN_POINT('Ctrl Pts',(3.15405075658949,7.16443384860501,2.35857787116297));
#9919=CARTESIAN_POINT('Ctrl Pts',(3.4489408371573,7.10714218193936,1.92806508852736));
#9920=CARTESIAN_POINT('Ctrl Pts',(3.85268394971518,6.99255884860513,0.981749147077123));
#9921=CARTESIAN_POINT('Ctrl Pts',(3.96134230903857,6.93526718193912,0.466303458167944));
#9922=CARTESIAN_POINT('Ctrl Pts',(3.97221287455602,6.82068384860537,-0.572196477765365));
#9923=CARTESIAN_POINT('Ctrl Pts',(3.87438202444231,6.76339218193869,-1.09484214611198));
#9924=CARTESIAN_POINT('Ctrl Pts',(3.48329169702894,6.6488088486058,-2.06742387531521));
#9925=CARTESIAN_POINT('Ctrl Pts',(3.19015025959274,6.5915171819388,-2.51696245110363));
#9926=CARTESIAN_POINT('Ctrl Pts',(2.44977142947187,6.47693384860569,-3.27271458243633));
#9927=CARTESIAN_POINT('Ctrl Pts',(2.00279790455941,6.41964218193941,-3.57860337931556));
#9928=CARTESIAN_POINT('Ctrl Pts',(1.02059032892293,6.30505884860508,-3.99721329356667));
#9929=CARTESIAN_POINT('Ctrl Pts',(0.485727870620802,6.24776718193879,-4.10973388842147));
#9930=CARTESIAN_POINT('Ctrl Pts',(-0.591620890218261,6.1331838486057,-4.12060445397352));
#9931=CARTESIAN_POINT('Ctrl Pts',(-1.13368332795069,6.07589218193929,-4.01891136825983));
#9932=CARTESIAN_POINT('Ctrl Pts',(-2.14215669135443,5.9613088486052,-3.61295423922114));
#9933=CARTESIAN_POINT('Ctrl Pts',(-2.60815600939102,5.90401718193932,-3.30881408541235));
#9934=CARTESIAN_POINT('Ctrl Pts',(-3.39137840827869,5.78943384860516,-2.54096498778195));
#9935=CARTESIAN_POINT('Ctrl Pts',(-3.70826592147772,5.73214218193892,-2.07753072058528));
#9936=CARTESIAN_POINT('Ctrl Pts',(-4.14174263741426,5.61755884860556,-1.05943151077492));
#9937=CARTESIAN_POINT('Ctrl Pts',(-4.25812546780629,5.56026718193889,-0.505152283069884));
#9938=CARTESIAN_POINT('Ctrl Pts',(-4.26899603338911,5.44568384860559,0.611045302667398));
#9939=CARTESIAN_POINT('Ctrl Pts',(-4.16344071207717,5.38839218193887,1.17252450979444));
#9940=CARTESIAN_POINT('Ctrl Pts',(-3.74261678141353,5.27380884860562,2.21688950738861));
#9941=CARTESIAN_POINT('Ctrl Pts',(-3.4274779112251,5.21651718193883,2.69934956768717));
#9942=CARTESIAN_POINT('Ctrl Pts',(-2.63215854609891,5.10193384860566,3.5100422341123));
#9943=CARTESIAN_POINT('Ctrl Pts',(-2.15226353660435,5.04464218193881,3.83792846364419));
#9944=CARTESIAN_POINT('Ctrl Pts',(-1.0982726926337,4.93005884860567,4.28627198125755));
#9945=CARTESIAN_POINT('Ctrl Pts',(-0.524576695510519,4.87276718193882,4.40651704719262));
#9946=CARTESIAN_POINT('Ctrl Pts',(0.630469715108076,4.75818384860566,4.41738761280318));
#9947=CARTESIAN_POINT('Ctrl Pts',(1.21136569164331,4.70089218193903,4.30797005589403));
#9948=CARTESIAN_POINT('Ctrl Pts',(2.29162232341768,4.58630884860546,3.87227932360639));
#9949=CARTESIAN_POINT('Ctrl Pts',(2.79054312598678,4.529017181939,3.5461417370364));
#9950=CARTESIAN_POINT('Ctrl Pts',(3.62870605994246,4.41443384860549,2.72335210441731));
#9951=CARTESIAN_POINT('Ctrl Pts',(3.96759100581396,4.35714218193895,2.22699635262072));
#9952=CARTESIAN_POINT('Ctrl Pts',(4.43080132509753,4.24255884860554,1.13711387449518));
#9953=CARTESIAN_POINT('Ctrl Pts',(4.55490862657983,4.18526718193866,0.544001107941954));
#9954=CARTESIAN_POINT('Ctrl Pts',(4.56577919221637,4.07068384860583,-0.649894127539557));
#9955=CARTESIAN_POINT('Ctrl Pts',(4.45249939970698,4.01339218193886,-1.25020687350361));
#9956=CARTESIAN_POINT('Ctrl Pts',(4.00194186580315,3.89880884860562,-2.36635513943533));
#9957=CARTESIAN_POINT('Ctrl Pts',(3.66480556284339,3.84151718193895,-2.88173668429245));
#9958=CARTESIAN_POINT('Ctrl Pts',(2.81454566274002,3.72693384860553,-3.74736988576655));
#9959=CARTESIAN_POINT('Ctrl Pts',(2.30172916862896,3.66964218193904,-4.09725354798759));
#9960=CARTESIAN_POINT('Ctrl Pts',(1.17595505636478,3.55505884860545,-4.57533066893367));
#9961=CARTESIAN_POINT('Ctrl Pts',(0.563425520373289,3.4977671819386,-4.70330020596852));
#9962=CARTESIAN_POINT('Ctrl Pts',(-0.669318539970923,3.38318384860588,-4.71417077162809));
#9963=CARTESIAN_POINT('Ctrl Pts',(-1.28904805536363,3.32589218193878,-4.59702874352091));
#9964=CARTESIAN_POINT('Ctrl Pts',(-2.44108795545323,3.21130884860571,-4.13160440799895));
#9965=CARTESIAN_POINT('Ctrl Pts',(-2.97293024260301,3.15401718193919,-3.78346938864651));
#9966=CARTESIAN_POINT('Ctrl Pts',(-3.86603371158577,3.03943384860528,-2.90573922106659));
#9967=CARTESIAN_POINT('Ctrl Pts',(-4.22691609016478,2.98214218193882,-2.37646198463267));
#9968=CARTESIAN_POINT('Ctrl Pts',(-4.71986001276623,2.86755884860567,-1.21479623823893));
#9969=CARTESIAN_POINT('Ctrl Pts',(-4.8516917853577,2.81026718193854,-0.582849932796644));
#9970=CARTESIAN_POINT('Ctrl Pts',(-4.86256235103931,2.69568384860595,0.688742952394343));
#9971=CARTESIAN_POINT('Ctrl Pts',(-4.74155808733321,2.638392181939,1.32788923723221));
#9972=CARTESIAN_POINT('Ctrl Pts',(-4.26126695019637,2.52380884860549,2.5158207714626));
#9973=CARTESIAN_POINT('Ctrl Pts',(-3.90213321444713,2.46651718193888,3.06412380091759));
#9974=CARTESIAN_POINT('Ctrl Pts',(-2.99693277939567,2.3519338486056,3.98469753740094));
#9975=CARTESIAN_POINT('Ctrl Pts',(-2.45119480063163,2.29464218193882,4.35657863234452));
#9976=CARTESIAN_POINT('Ctrl Pts',(-1.2536374201178,2.18005884860566,4.86438935659626));
#9977=CARTESIAN_POINT('Ctrl Pts',(-0.602274345215141,2.12276718193851,5.00008336474837));
#9978=CARTESIAN_POINT('Ctrl Pts',(0.708167364812911,2.00818384860598,5.01095393044905));
#9979=CARTESIAN_POINT('Ctrl Pts',(1.36673041909958,1.95089218193886,4.8860874311467));
#9980=CARTESIAN_POINT('Ctrl Pts',(2.59055358747315,1.83630884860562,4.39092949239261));
#9981=CARTESIAN_POINT('Ctrl Pts',(3.15531735923718,1.77901718193906,4.02079704024371));
#9982=CARTESIAN_POINT('Ctrl Pts',(4.10336136321113,1.66443384860542,3.08812633772876));
#9983=CARTESIAN_POINT('Ctrl Pts',(4.48624117452488,1.60714218193865,2.52592761663043));
#9984=CARTESIAN_POINT('Ctrl Pts',(5.00891870042567,1.49255884860583,1.29247860199682));
#9985=CARTESIAN_POINT('Ctrl Pts',(5.14847494413939,1.43526718193912,0.621698757625503));
#9986=CARTESIAN_POINT('Ctrl Pts',(5.15934550985844,1.32068384860537,-0.727591777223308));
#9987=CARTESIAN_POINT('Ctrl Pts',(5.0306167749558,1.26339218193915,-1.40557160097741));
#9988=CARTESIAN_POINT('Ctrl Pts',(4.52059203459322,1.14880884860534,-2.66528640347329));
#9989=CARTESIAN_POINT('Ctrl Pts',(4.13946086604337,1.09151718193863,-3.24651091755445));
#9990=CARTESIAN_POINT('Ctrl Pts',(3.17931989605881,0.976933848605856,-4.22202518902362));
#9991=CARTESIAN_POINT('Ctrl Pts',(2.60066043261983,0.919642181938648,-4.61590371671046));
#9992=CARTESIAN_POINT('Ctrl Pts',(1.33131978388528,0.805058848605838,-5.15344804424985));
#9993=CARTESIAN_POINT('Ctrl Pts',(0.641123170036348,0.747767181938915,-5.29686652353057));
#9994=CARTESIAN_POINT('Ctrl Pts',(-0.747016189634228,0.633183848605571,
-5.30773708926766));
#9995=CARTESIAN_POINT('Ctrl Pts',(-1.44441278286383,0.575892181939075,-5.17514611876316));
#9996=CARTESIAN_POINT('Ctrl Pts',(-2.74001921946479,0.46130884860541,-4.65025457679559));
#9997=CARTESIAN_POINT('Ctrl Pts',(-3.33770446803392,0.404017181938794,-4.25812469903555));
#9998=CARTESIAN_POINT('Ctrl Pts',(-3.83919674535392,0.346725515272242,-3.76431907311593));
#9999=CARTESIAN_POINT('Ctrl Pts',(-2.12557398216503,11.,-2.11821519670878));
#10000=CARTESIAN_POINT('Ctrl Pts',(-2.41159176945725,10.9427083333325,-1.84872226348015));
#10001=CARTESIAN_POINT('Ctrl Pts',(-2.6456803034859,10.8854166666664,-1.52067018109149));
#10002=CARTESIAN_POINT('Ctrl Pts',(-2.97162798586693,10.7708333333336,-0.794830755283512));
#10003=CARTESIAN_POINT('Ctrl Pts',(-3.06332306119362,10.7135416666669,-0.397314139662748));
#10004=CARTESIAN_POINT('Ctrl Pts',(-3.08669273082211,10.5989583333331,0.407721033857582));
#10005=CARTESIAN_POINT('Ctrl Pts',(-3.01831935235521,10.5416666666666,0.814922877330024));
#10006=CARTESIAN_POINT('Ctrl Pts',(-2.728119788021,10.4270833333334,1.57659449107116));
#10007=CARTESIAN_POINT('Ctrl Pts',(-2.50637194487625,10.3697916666664,1.93074976622997));
#10008=CARTESIAN_POINT('Ctrl Pts',(-1.93991583267103,10.2552083333337,2.53025558222984));
#10009=CARTESIAN_POINT('Ctrl Pts',(-1.59540299717169,10.1979166666664,2.77534284559852));
#10010=CARTESIAN_POINT('Ctrl Pts',(-0.833671937081177,10.0833333333336,
3.11615732976406));
#10011=CARTESIAN_POINT('Ctrl Pts',(-0.416738552178117,10.0260416666666,
3.21171464055396));
#10012=CARTESIAN_POINT('Ctrl Pts',(0.427145446372979,9.91145833333345,3.23508431026218));
#10013=CARTESIAN_POINT('Ctrl Pts',(0.853764059103477,9.85416666666669,3.16284869617602));
#10014=CARTESIAN_POINT('Ctrl Pts',(1.65132730717562,9.73958333333332,2.85778233020993));
#10015=CARTESIAN_POINT('Ctrl Pts',(2.02194332446279,9.68229166666673,2.62503577071995));
#10016=CARTESIAN_POINT('Ctrl Pts',(2.64891940812677,9.56770833333328,2.03110939095704));
#10017=CARTESIAN_POINT('Ctrl Pts',(2.9050053877204,9.51041666666666,1.67013581324179));
#10018=CARTESIAN_POINT('Ctrl Pts',(3.26068667365192,9.39583333333334,0.872513118888943));
#10019=CARTESIAN_POINT('Ctrl Pts',(3.36010621991895,9.3385416666664,0.436162964680591));
#10020=CARTESIAN_POINT('Ctrl Pts',(3.38347588969759,9.22395833333361,-0.446569858875482));
#10021=CARTESIAN_POINT('Ctrl Pts',(3.30737803999626,9.16666666666689,-0.892605240889856));
#10022=CARTESIAN_POINT('Ctrl Pts',(2.98744487239941,9.05208333333312,-1.72606012326716));
#10023=CARTESIAN_POINT('Ctrl Pts',(2.74369959655829,8.99479166666641,-2.11313688270712));
#10024=CARTESIAN_POINT('Ctrl Pts',(2.1223029492484,8.8802083333336,-2.76758323401219));
#10025=CARTESIAN_POINT('Ctrl Pts',(1.74486862930228,8.82291666666647,-3.03466792985017));
#10026=CARTESIAN_POINT('Ctrl Pts',(0.911354300706321,8.70833333333354,-3.40521601753191));
#10027=CARTESIAN_POINT('Ctrl Pts',(0.455587377172263,8.6510416666665,-3.5084977992874));
#10028=CARTESIAN_POINT('Ctrl Pts',(-0.465994271367186,8.53645833333351,
-3.53186746912954));
#10029=CARTESIAN_POINT('Ctrl Pts',(-0.93144642268745,8.47916666666683,-3.45190738381581));
#10030=CARTESIAN_POINT('Ctrl Pts',(-1.80079293934749,8.36458333333318,-3.11710741458959));
#10031=CARTESIAN_POINT('Ctrl Pts',(-2.20433044096071,8.30729166666683,-2.86236342239196));
#10032=CARTESIAN_POINT('Ctrl Pts',(-2.88624705988836,8.1927083333332,-2.21349650754444));
#10033=CARTESIAN_POINT('Ctrl Pts',(-3.1643304719878,8.13541666666656,-1.81960144535507));
#10034=CARTESIAN_POINT('Ctrl Pts',(-3.54974536140404,8.02083333333345,-0.950195482531384));
#10035=CARTESIAN_POINT('Ctrl Pts',(-3.65688937865929,7.96354166666637,-0.475011789653154));
#10036=CARTESIAN_POINT('Ctrl Pts',(-3.68025904855805,7.84895833333365,0.485418683848109));
#10037=CARTESIAN_POINT('Ctrl Pts',(-3.59643672763413,7.79166666666665,0.970287604495667));
#10038=CARTESIAN_POINT('Ctrl Pts',(-3.246769956781,7.67708333333337,1.8755257554172));
#10039=CARTESIAN_POINT('Ctrl Pts',(-2.98102724821984,7.61979166666659,2.29552399922486));
#10040=CARTESIAN_POINT('Ctrl Pts',(-2.30469006584627,7.50520833333343,3.00491088575395));
#10041=CARTESIAN_POINT('Ctrl Pts',(-1.89433426139971,7.44791666666668,3.29399301413121));
#10042=CARTESIAN_POINT('Ctrl Pts',(-0.989036664364609,7.33333333333333,
3.69427470527038));
#10043=CARTESIAN_POINT('Ctrl Pts',(-0.49443620212397,7.27604166666629,3.80528095803426));
#10044=CARTESIAN_POINT('Ctrl Pts',(0.50484309631896,7.16145833333372,3.82865062798349));
#10045=CARTESIAN_POINT('Ctrl Pts',(1.00912878631411,7.10416666666678,3.74096607145172));
#10046=CARTESIAN_POINT('Ctrl Pts',(1.95025857147667,6.98958333333323,3.37643249897315));
#10047=CARTESIAN_POINT('Ctrl Pts',(2.38671755749636,6.93229166666724,3.09969107404422));
#10048=CARTESIAN_POINT('Ctrl Pts',(3.12357471161222,6.81770833333277,2.39588362415159));
#10049=CARTESIAN_POINT('Ctrl Pts',(3.42365555628099,6.76041666666712,1.96906707743673));
#10050=CARTESIAN_POINT('Ctrl Pts',(3.83880404913035,6.64583333333289,1.02787784620545));
#10051=CARTESIAN_POINT('Ctrl Pts',(3.95367253741186,6.58854166666688,0.51386061458762));
#10052=CARTESIAN_POINT('Ctrl Pts',(3.97704220740629,6.47395833333313,-0.524267508782646));
#10053=CARTESIAN_POINT('Ctrl Pts',(3.88549541526866,6.41666666666645,-1.04796996813959));
#10054=CARTESIAN_POINT('Ctrl Pts',(3.50609504116593,6.30208333333356,-2.02499138752914));
#10055=CARTESIAN_POINT('Ctrl Pts',(3.2183548998624,6.24479166666656,-2.47791111577681));
#10056=CARTESIAN_POINT('Ctrl Pts',(2.48707718246311,6.13020833333345,-3.24223853746153));
#10057=CARTESIAN_POINT('Ctrl Pts',(2.04379989346725,6.07291666666717,-3.55331809843599));
#10058=CARTESIAN_POINT('Ctrl Pts',(1.06671902805278,5.95833333333284,-3.9833333929851));
#10059=CARTESIAN_POINT('Ctrl Pts',(0.533285027040294,5.90104166666655,-4.10206411679133));
#10060=CARTESIAN_POINT('Ctrl Pts',(-0.543691921235359,5.78645833333346,
-4.12543378682723));
#10061=CARTESIAN_POINT('Ctrl Pts',(-1.08681114997705,5.72916666666705,-4.03002475908303));
#10062=CARTESIAN_POINT('Ctrl Pts',(-2.0997242035696,5.61458333333296,-3.63575758336128));
#10063=CARTESIAN_POINT('Ctrl Pts',(-2.56910467406188,5.55729166666709,-3.33701872567955));
#10064=CARTESIAN_POINT('Ctrl Pts',(-3.36090236330622,5.44270833333292,-2.57827074077566));
#10065=CARTESIAN_POINT('Ctrl Pts',(-3.68298064059524,5.38541666666669,-2.11853270949184));
#10066=CARTESIAN_POINT('Ctrl Pts',(-4.12786273683561,5.27083333333332,-1.10556020990605));
#10067=CARTESIAN_POINT('Ctrl Pts',(-4.25045569617289,5.21354166666665,-0.552709439489368));
#10068=CARTESIAN_POINT('Ctrl Pts',(-4.27382536624608,5.09895833333335,0.563116333684488));
#10069=CARTESIAN_POINT('Ctrl Pts',(-4.17455410289751,5.04166666666663,1.12565233181968));
#10070=CARTESIAN_POINT('Ctrl Pts',(-3.76542012555652,4.92708333333338,2.17445701960491));
#10071=CARTESIAN_POINT('Ctrl Pts',(-3.45568255149002,4.86979166666659,2.66029823235588));
#10072=CARTESIAN_POINT('Ctrl Pts',(-2.6694642990949,4.75520833333342,3.47956618914197));
#10073=CARTESIAN_POINT('Ctrl Pts',(-2.19326552550957,4.69791666666658,3.81264318275876));
#10074=CARTESIAN_POINT('Ctrl Pts',(-1.14440139176617,4.58333333333343,4.27239208068185));
#10075=CARTESIAN_POINT('Ctrl Pts',(-0.572133851929879,4.52604166666658,
4.39884727555618));
#10076=CARTESIAN_POINT('Ctrl Pts',(0.582540746125043,4.41145833333343,4.42221694566319));
#10077=CARTESIAN_POINT('Ctrl Pts',(1.16449351366757,4.35416666666679,4.31908344671154));
#10078=CARTESIAN_POINT('Ctrl Pts',(2.24918983563495,4.23958333333322,3.89508266775222));
#10079=CARTESIAN_POINT('Ctrl Pts',(2.75149179065353,4.18229166666676,3.57434637729919));
#10080=CARTESIAN_POINT('Ctrl Pts',(3.59823001497408,4.06770833333325,2.76065785741543));
#10081=CARTESIAN_POINT('Ctrl Pts',(3.94230572492611,4.01041666666671,2.26799834152485));
#10082=CARTESIAN_POINT('Ctrl Pts',(4.41692142452426,3.8958333333333,1.18324257362874));
#10083=CARTESIAN_POINT('Ctrl Pts',(4.54723885494094,3.83854166666642,0.591558264361257));
#10084=CARTESIAN_POINT('Ctrl Pts',(4.57060852507883,3.72395833333359,-0.601965158556466));
#10085=CARTESIAN_POINT('Ctrl Pts',(4.46361279052205,3.66666666666662,-1.20333469552689));
#10086=CARTESIAN_POINT('Ctrl Pts',(4.02474520995143,3.55208333333339,-2.32392265165357));
#10087=CARTESIAN_POINT('Ctrl Pts',(3.69301020310442,3.49479166666671,-2.84268534895739));
#10088=CARTESIAN_POINT('Ctrl Pts',(2.85185141573989,3.38020833333329,-3.71689384079999));
#10089=CARTESIAN_POINT('Ctrl Pts',(2.34273115753217,3.3229166666668,-4.07196826709743));
#10090=CARTESIAN_POINT('Ctrl Pts',(1.22208375549926,3.20833333333321,-4.56145076836271));
#10091=CARTESIAN_POINT('Ctrl Pts',(0.610982676792531,3.15104166666636,-4.6956304343271));
#10092=CARTESIAN_POINT('Ctrl Pts',(-0.621389570987771,3.03645833333365,
-4.71900010449308));
#10093=CARTESIAN_POINT('Ctrl Pts',(-1.24217587738614,2.97916666666654,-4.60814213433379));
#10094=CARTESIAN_POINT('Ctrl Pts',(-2.39865546767225,2.86458333333347,-4.15440775214941));
#10095=CARTESIAN_POINT('Ctrl Pts',(-2.93387890726637,2.80729166666695,-3.81167402890586));
#10096=CARTESIAN_POINT('Ctrl Pts',(-3.83555766662078,2.69270833333305,-2.94304497406814));
#10097=CARTESIAN_POINT('Ctrl Pts',(-4.20163080927273,2.63541666666658,-2.41746397353493));
#10098=CARTESIAN_POINT('Ctrl Pts',(-4.70598011219716,2.52083333333343,-1.26092493737436));
#10099=CARTESIAN_POINT('Ctrl Pts',(-4.84402201371418,2.4635416666663,-0.630407089215845));
#10100=CARTESIAN_POINT('Ctrl Pts',(-4.86739168390641,2.34895833333371,0.64081398341115));
#10101=CARTESIAN_POINT('Ctrl Pts',(-4.75267147814405,2.29166666666676,1.28101705925391));
#10102=CARTESIAN_POINT('Ctrl Pts',(-4.28407029434887,2.17708333333325,2.47338828368244));
#10103=CARTESIAN_POINT('Ctrl Pts',(-3.93033785470491,2.11979166666664,3.0250724655795));
#10104=CARTESIAN_POINT('Ctrl Pts',(-3.0342385323988,2.00520833333337,3.95422149243741));
#10105=CARTESIAN_POINT('Ctrl Pts',(-2.49219678953305,1.94791666666658,4.33129335145034));
#10106=CARTESIAN_POINT('Ctrl Pts',(-1.29976611925407,1.83333333333343,4.85050945602931));
#10107=CARTESIAN_POINT('Ctrl Pts',(-0.6498315016342,1.77604166666627,4.99241359310244));
#10108=CARTESIAN_POINT('Ctrl Pts',(0.660238395829575,1.66145833333374,5.01578326331855));
#10109=CARTESIAN_POINT('Ctrl Pts',(1.31985824112059,1.60416666666663,4.89720082195578));
#10110=CARTESIAN_POINT('Ctrl Pts',(2.54812109969368,1.48958333333338,4.41373283654687));
#10111=CARTESIAN_POINT('Ctrl Pts',(3.1162660238978,1.43229166666683,4.04900168050008));
#10112=CARTESIAN_POINT('Ctrl Pts',(4.07288531824889,1.31770833333318,3.1254320907333));
#10113=CARTESIAN_POINT('Ctrl Pts',(4.460955893629,1.26041666666641,2.56692960553103));
#10114=CARTESIAN_POINT('Ctrl Pts',(4.99503879986042,1.1458333333336,1.33860730113391));
#10115=CARTESIAN_POINT('Ctrl Pts',(5.14080517249185,1.08854166666688,0.669255914044516));
#10116=CARTESIAN_POINT('Ctrl Pts',(5.16417484272955,0.973958333333134,-0.679662808239928));
#10117=CARTESIAN_POINT('Ctrl Pts',(5.04173016576313,0.916666666666909,-1.35869942299763));
#10118=CARTESIAN_POINT('Ctrl Pts',(4.54339537874923,0.8020833333331,-2.62285391569459));
#10119=CARTESIAN_POINT('Ctrl Pts',(4.16766550629842,0.744791666666392,-3.20745958221381));
#10120=CARTESIAN_POINT('Ctrl Pts',(3.21662564906467,0.630208333333619,-4.19154914406263));
#10121=CARTESIAN_POINT('Ctrl Pts',(2.6416624215197,0.572916666666411,-4.59061843581319));
#10122=CARTESIAN_POINT('Ctrl Pts',(1.3774484830231,0.4583333333336,-5.13956814368599));
#10123=CARTESIAN_POINT('Ctrl Pts',(0.688680326455284,0.401041666666677,
-5.28919675188146));
#10124=CARTESIAN_POINT('Ctrl Pts',(-0.69908722065077,0.286458333333334,
-5.31256642214034));
#10125=CARTESIAN_POINT('Ctrl Pts',(-1.39754060488348,0.229166666666838,
-5.1862595095691));
#10126=CARTESIAN_POINT('Ctrl Pts',(-2.69758673168668,0.114583333333173,
-4.67305792095299));
#10127=CARTESIAN_POINT('Ctrl Pts',(-3.29865313262765,0.0572916666665569,
-4.28632933922004));
#10128=CARTESIAN_POINT('Ctrl Pts',(-3.80443305520312,5.20417042793042E-15,
-3.79707426974638));
#10129=CARTESIAN_POINT('Ctrl Pts',(-2.09081029201422,10.6532744847278,-2.15097039333923));
#10130=CARTESIAN_POINT('Ctrl Pts',(-2.38111572464286,10.5959828180603,-1.88602801664143));
#10131=CARTESIAN_POINT('Ctrl Pts',(-2.6203950226392,10.5386911513942,-1.56167217001419));
#10132=CARTESIAN_POINT('Ctrl Pts',(-2.9577480852525,10.4241078180613,-0.840959454398505));
#10133=CARTESIAN_POINT('Ctrl Pts',(-3.05565328959838,10.3668161513947,-0.444871296083357));
#10134=CARTESIAN_POINT('Ctrl Pts',(-3.09152206364091,10.2522328180609,0.359792064875797));
#10135=CARTESIAN_POINT('Ctrl Pts',(-3.02943274321019,10.1949411513944,0.768050699368431));
#10136=CARTESIAN_POINT('Ctrl Pts',(-2.75092313212936,10.0803578180611,1.53416200327429));
#10137=CARTESIAN_POINT('Ctrl Pts',(-2.53457658516751,10.0230661513941,1.89169843092347));
#10138=CARTESIAN_POINT('Ctrl Pts',(-1.97722158564067,9.90848281806141,2.49977953723472));
#10139=CARTESIAN_POINT('Ctrl Pts',(-1.6364049860914,9.8511911513942,2.75005756474531));
#10140=CARTESIAN_POINT('Ctrl Pts',(-0.879800636199156,9.73660781806133,
3.10227742915614));
#10141=CARTESIAN_POINT('Ctrl Pts',(-0.46429570859848,9.67931615139432,3.2040448689519));
#10142=CARTESIAN_POINT('Ctrl Pts',(0.379216477390949,9.56473281806121,3.2399136430878));
#10143=CARTESIAN_POINT('Ctrl Pts',(0.806891881139562,9.50744115139445,3.17396208702488));
#10144=CARTESIAN_POINT('Ctrl Pts',(1.60889481938107,9.39285781806108,2.8805856743244));
#10145=CARTESIAN_POINT('Ctrl Pts',(1.98289198915187,9.33556615139449,2.65324041100648));
#10146=CARTESIAN_POINT('Ctrl Pts',(2.61844336313606,9.22098281806105,2.06841514393141));
#10147=CARTESIAN_POINT('Ctrl Pts',(2.87972010686153,9.16369115139443,1.71113780215899));
#10148=CARTESIAN_POINT('Ctrl Pts',(3.24680677304967,9.0491078180611,0.918641818009435));
#10149=CARTESIAN_POINT('Ctrl Pts',(3.35243644831083,8.99181615139416,0.483720121100777));
#10150=CARTESIAN_POINT('Ctrl Pts',(3.38830522252928,8.87723281806137,-0.398640889893273));
#10151=CARTESIAN_POINT('Ctrl Pts',(3.31849143083958,8.81994115139465,-0.845733062923796));
#10152=CARTESIAN_POINT('Ctrl Pts',(3.01024821651943,8.70535781806088,-1.68362763547476));
#10153=CARTESIAN_POINT('Ctrl Pts',(2.77190423684068,8.64806615139417,-2.0740855473923));
#10154=CARTESIAN_POINT('Ctrl Pts',(2.15960870222691,8.53348281806136,-2.73710718902539));
#10155=CARTESIAN_POINT('Ctrl Pts',(1.78587061821714,8.47619115139423,-3.00938264898613));
#10156=CARTESIAN_POINT('Ctrl Pts',(0.957482999829145,8.36160781806131,-3.39133611693482));
#10157=CARTESIAN_POINT('Ctrl Pts',(0.503144533592307,8.30431615139426,-3.50082802767378));
#10158=CARTESIAN_POINT('Ctrl Pts',(-0.418065302384836,8.18973281806127,
-3.53669680196673));
#10159=CARTESIAN_POINT('Ctrl Pts',(-0.884574244719486,8.13244115139459,
-3.4630207746542));
#10160=CARTESIAN_POINT('Ctrl Pts',(-1.75836045155699,8.01785781806094,-3.13991075871454));
#10161=CARTESIAN_POINT('Ctrl Pts',(-2.16527910564236,7.96056615139459,-2.89056806267063));
#10162=CARTESIAN_POINT('Ctrl Pts',(-2.85577101490508,7.84598281806096,-2.25080226052667));
#10163=CARTESIAN_POINT('Ctrl Pts',(-3.13904519111934,7.78869115139432,-1.8606034342679));
#10164=CARTESIAN_POINT('Ctrl Pts',(-3.53586546081137,7.67410781806122,-0.996324181656243));
#10165=CARTESIAN_POINT('Ctrl Pts',(-3.64921960704095,7.61681615139413,-0.52256894607304));
#10166=CARTESIAN_POINT('Ctrl Pts',(-3.68508838139996,7.50223281806141,0.437489714865601));
#10167=CARTESIAN_POINT('Ctrl Pts',(-3.60755011846799,7.44494115139464,0.923415426526065));
#10168=CARTESIAN_POINT('Ctrl Pts',(-3.26957330091048,7.33035781806089,1.83309326762834));
#10169=CARTESIAN_POINT('Ctrl Pts',(-3.00923188849514,7.27306615139411,2.25647266390339));
#10170=CARTESIAN_POINT('Ctrl Pts',(-2.34199581883187,7.15848281806142,2.9744348407738));
#10171=CARTESIAN_POINT('Ctrl Pts',(-1.93533625031079,7.10119115139444,3.26870773325855));
#10172=CARTESIAN_POINT('Ctrl Pts',(-1.03516536349121,6.98660781806109,3.68039480468192));
#10173=CARTESIAN_POINT('Ctrl Pts',(-0.541993358543724,6.92931615139405,
3.79761118641148));
#10174=CARTESIAN_POINT('Ctrl Pts',(0.45691412733632,6.81473281806148,3.83347996082984));
#10175=CARTESIAN_POINT('Ctrl Pts',(0.962256608343087,6.75744115139454,3.75207946228173));
#10176=CARTESIAN_POINT('Ctrl Pts',(1.90782608368924,6.64285781806099,3.39923584310647));
#10177=CARTESIAN_POINT('Ctrl Pts',(2.34766622217201,6.585566151395,3.12789571431651));
#10178=CARTESIAN_POINT('Ctrl Pts',(3.09309866663495,6.47098281806054,2.4331893771402));
#10179=CARTESIAN_POINT('Ctrl Pts',(3.39837027540469,6.41369115139488,2.01006906634609));
#10180=CARTESIAN_POINT('Ctrl Pts',(3.82492414854553,6.29910781806065,1.07400654533378));
#10181=CARTESIAN_POINT('Ctrl Pts',(3.94600276578516,6.24181615139464,0.561417771007294));
#10182=CARTESIAN_POINT('Ctrl Pts',(3.98187154025657,6.1272328180609,-0.476338539799928));
#10183=CARTESIAN_POINT('Ctrl Pts',(3.89660880609501,6.06994115139421,-1.00109779016719));
#10184=CARTESIAN_POINT('Ctrl Pts',(3.52889838530292,5.95535781806132,-1.98255889974307));
#10185=CARTESIAN_POINT('Ctrl Pts',(3.24655954013207,5.89806615139432,-2.43885978044999));
#10186=CARTESIAN_POINT('Ctrl Pts',(2.52438293545435,5.78348281806122,-3.21176249248673));
#10187=CARTESIAN_POINT('Ctrl Pts',(2.08480188237509,5.72619115139493,-3.52803281755643));
#10188=CARTESIAN_POINT('Ctrl Pts',(1.11284772718263,5.6116078180606,-3.96945349240354));
#10189=CARTESIAN_POINT('Ctrl Pts',(0.580842183459787,5.55431615139431,-4.0943943451612));
#10190=CARTESIAN_POINT('Ctrl Pts',(-0.495762952252458,5.43973281806122,
-4.13026311968094));
#10191=CARTESIAN_POINT('Ctrl Pts',(-1.03993897200342,5.38244115139481,-4.04113814990623));
#10192=CARTESIAN_POINT('Ctrl Pts',(-2.05729171578477,5.26785781806072,-3.65856092750142));
#10193=CARTESIAN_POINT('Ctrl Pts',(-2.53005333873273,5.21056615139485,-3.36522336594676));
#10194=CARTESIAN_POINT('Ctrl Pts',(-3.33042631833374,5.09598281806069,-2.61557649376936));
#10195=CARTESIAN_POINT('Ctrl Pts',(-3.65769535971276,5.03869115139445,-2.1595346983984));
#10196=CARTESIAN_POINT('Ctrl Pts',(-4.11398283625697,4.92410781806109,-1.15168890903718));
#10197=CARTESIAN_POINT('Ctrl Pts',(-4.24278592453948,4.86681615139442,-0.600266595908851));
#10198=CARTESIAN_POINT('Ctrl Pts',(-4.27865469910306,4.75223281806112,0.515187364701578));
#10199=CARTESIAN_POINT('Ctrl Pts',(-4.18566749371785,4.69494115139439,1.07878015384492));
#10200=CARTESIAN_POINT('Ctrl Pts',(-3.78822346969952,4.58035781806114,2.13202453182121));
#10201=CARTESIAN_POINT('Ctrl Pts',(-3.48388719175493,4.52306615139435,2.62124689702459));
#10202=CARTESIAN_POINT('Ctrl Pts',(-2.70677005209088,4.40848281806118,3.44909014417165));
#10203=CARTESIAN_POINT('Ctrl Pts',(-2.2342675144148,4.35119115139434,3.78735790187333));
#10204=CARTESIAN_POINT('Ctrl Pts',(-1.19053009089864,4.2366078180612,4.25851218010615));
#10205=CARTESIAN_POINT('Ctrl Pts',(-0.61969100834924,4.17931615139434,4.39117750391975));
#10206=CARTESIAN_POINT('Ctrl Pts',(0.53461177714201,4.06473281806119,4.42704627852319));
#10207=CARTESIAN_POINT('Ctrl Pts',(1.11762133569182,4.00744115139456,4.33019683752905));
#10208=CARTESIAN_POINT('Ctrl Pts',(2.20675734785223,3.89285781806098,3.91788601189805));
#10209=CARTESIAN_POINT('Ctrl Pts',(2.71244045532029,3.83556615139452,3.60255101756198));
#10210=CARTESIAN_POINT('Ctrl Pts',(3.56775397000571,3.72098281806102,2.79796361041354));
#10211=CARTESIAN_POINT('Ctrl Pts',(3.91702044403826,3.66369115139447,2.30900033042897));
#10212=CARTESIAN_POINT('Ctrl Pts',(4.40304152395098,3.54910781806106,1.22937127276231));
#10213=CARTESIAN_POINT('Ctrl Pts',(4.53956908330205,3.49181615139418,0.63911542078056));
#10214=CARTESIAN_POINT('Ctrl Pts',(4.5754378579413,3.37723281806136,-0.554036189573376));
#10215=CARTESIAN_POINT('Ctrl Pts',(4.47472618133712,3.31994115139439,-1.15646251755018));
#10216=CARTESIAN_POINT('Ctrl Pts',(4.0475485540997,3.20535781806115,-2.28149016387182));
#10217=CARTESIAN_POINT('Ctrl Pts',(3.72121484336545,3.14806615139448,-2.80363401362233));
#10218=CARTESIAN_POINT('Ctrl Pts',(2.88915716873977,3.03348281806106,-3.68641779583343));
#10219=CARTESIAN_POINT('Ctrl Pts',(2.38373314643537,2.97619115139456,-4.04668298620726));
#10220=CARTESIAN_POINT('Ctrl Pts',(1.26821245463375,2.86160781806097,-4.54757086779175));
#10221=CARTESIAN_POINT('Ctrl Pts',(0.658539833211772,2.80431615139412,-4.68796066268569));
#10222=CARTESIAN_POINT('Ctrl Pts',(-0.573460602004618,2.68973281806141,
-4.72382943735807));
#10223=CARTESIAN_POINT('Ctrl Pts',(-1.19530369940865,2.6324411513943,-4.61925552514667));
#10224=CARTESIAN_POINT('Ctrl Pts',(-2.35622297989128,2.51785781806124,-4.17721109629987));
#10225=CARTESIAN_POINT('Ctrl Pts',(-2.89482757192974,2.46056615139471,-3.83987866916521));
#10226=CARTESIAN_POINT('Ctrl Pts',(-3.8050816216558,2.34598281806081,-2.98035072706969));
#10227=CARTESIAN_POINT('Ctrl Pts',(-4.17634552838067,2.28869115139434,-2.4584659624372));
#10228=CARTESIAN_POINT('Ctrl Pts',(-4.6921002116281,2.1741078180612,-1.30705363650978));
#10229=CARTESIAN_POINT('Ctrl Pts',(-4.83635224207065,2.11681615139406,-0.677964245635046));
#10230=CARTESIAN_POINT('Ctrl Pts',(-4.87222101677351,2.00223281806147,0.592885014427957));
#10231=CARTESIAN_POINT('Ctrl Pts',(-4.76378486895489,1.94494115139452,1.23414488127561));
#10232=CARTESIAN_POINT('Ctrl Pts',(-4.30687363850137,1.83035781806102,2.43095579590227));
#10233=CARTESIAN_POINT('Ctrl Pts',(-3.95854249496268,1.77306615139441,2.98602113024142));
#10234=CARTESIAN_POINT('Ctrl Pts',(-3.07154428540192,1.65848281806113,3.92374544747388));
#10235=CARTESIAN_POINT('Ctrl Pts',(-2.53319877843447,1.60119115139435,4.30600807055617));
#10236=CARTESIAN_POINT('Ctrl Pts',(-1.34589481839034,1.48660781806119,4.83662955546236));
#10237=CARTESIAN_POINT('Ctrl Pts',(-0.697388658053259,1.42931615139403,
4.9847438214565));
#10238=CARTESIAN_POINT('Ctrl Pts',(0.61230942684624,1.3147328180615,5.02061259618806));
#10239=CARTESIAN_POINT('Ctrl Pts',(1.27298606314159,1.25744115139439,4.90831421276487));
#10240=CARTESIAN_POINT('Ctrl Pts',(2.50568861191421,1.14285781806115,4.43653618070112));
#10241=CARTESIAN_POINT('Ctrl Pts',(3.07721468855841,1.08556615139459,4.07720632075644));
#10242=CARTESIAN_POINT('Ctrl Pts',(4.04240927328666,0.970982818060947,3.16273784373784));
#10243=CARTESIAN_POINT('Ctrl Pts',(4.43567061273313,0.913691151394175,2.60793159443164));
#10244=CARTESIAN_POINT('Ctrl Pts',(4.98115889929517,0.79910781806136,1.384736000271));
#10245=CARTESIAN_POINT('Ctrl Pts',(5.13313540084431,0.741816151394642,0.716813070463529));
#10246=CARTESIAN_POINT('Ctrl Pts',(5.16900417560066,0.627232818060896,-0.631733839256547));
#10247=CARTESIAN_POINT('Ctrl Pts',(5.05284355657047,0.569941151394671,-1.31182724501786));
#10248=CARTESIAN_POINT('Ctrl Pts',(4.56619872290524,0.455357818060863,-2.5804214279159));
#10249=CARTESIAN_POINT('Ctrl Pts',(4.19587014655347,0.398066151394155,-3.16840824687318));
#10250=CARTESIAN_POINT('Ctrl Pts',(3.25393140207052,0.283482818061382,-4.16107309910165));
#10251=CARTESIAN_POINT('Ctrl Pts',(2.68266441041957,0.226191151394174,-4.56533315491593));
#10252=CARTESIAN_POINT('Ctrl Pts',(1.42357718216092,0.111607818061363,-5.12568824312213));
#10253=CARTESIAN_POINT('Ctrl Pts',(0.736237482874218,0.0543161513944401,
-5.28152698023234));
#10254=CARTESIAN_POINT('Ctrl Pts',(-0.651158251667311,-0.0602671819389035,
-5.31739575501303));
#10255=CARTESIAN_POINT('Ctrl Pts',(-1.35066842690312,-0.117558848605399,
-5.19737290037505));
#10256=CARTESIAN_POINT('Ctrl Pts',(-2.65515424390857,-0.232142181939065,
-4.69586126511038));
#10257=CARTESIAN_POINT('Ctrl Pts',(-3.25960179722137,-0.28943384860568,
-4.31453397940454));
#10258=CARTESIAN_POINT('Ctrl Pts',(-3.76966936505231,-0.346725515272232,
-3.82982946637684));
#10259=CARTESIAN_POINT('Ctrl Pts',(-2.33082945277919,10.6532744847278,-2.40570712501662));
#10260=CARTESIAN_POINT('Ctrl Pts',(-2.65447984657204,10.5959828180603,-2.10934631273779));
#10261=CARTESIAN_POINT('Ctrl Pts',(-2.92084392795166,10.5386911513942,-1.74695427828554));
#10262=CARTESIAN_POINT('Ctrl Pts',(-3.29576381367816,10.4241078180613,-0.942666738728405));
#10263=CARTESIAN_POINT('Ctrl Pts',(-3.40413627693083,10.3668161513947,-0.501072825334149));
#10264=CARTESIAN_POINT('Ctrl Pts',(-3.44272956946446,10.2522328180609,0.39517980573707));
#10265=CARTESIAN_POINT('Ctrl Pts',(-3.37289643675743,10.1949411513944,0.849485922498689));
#10266=CARTESIAN_POINT('Ctrl Pts',(-3.06185425628309,10.0803578180611,1.70125730657109));
#10267=CARTESIAN_POINT('Ctrl Pts',(-2.82073175110235,10.0230661513941,2.0983726319291));
#10268=CARTESIAN_POINT('Ctrl Pts',(-2.2005398830606,9.90848281806141,2.77314365775904));
#10269=CARTESIAN_POINT('Ctrl Pts',(-1.82168709441022,9.8511911513942,3.05050647003645));
#10270=CARTESIAN_POINT('Ctrl Pts',(-0.98150792048159,9.73660781806133,3.44029315760313));
#10271=CARTESIAN_POINT('Ctrl Pts',(-0.520497237899657,9.67931615139432,
3.55252785628273));
#10272=CARTESIAN_POINT('Ctrl Pts',(0.41460421830261,9.56473281806121,3.59112114891296));
#10273=CARTESIAN_POINT('Ctrl Pts',(0.888327104224163,9.50744115139445,3.51742578058933));
#10274=CARTESIAN_POINT('Ctrl Pts',(1.77599012272354,9.39285781806108,3.19151679846092));
#10275=CARTESIAN_POINT('Ctrl Pts',(2.18956619012306,9.33556615139449,2.93939557697384));
#10276=CARTESIAN_POINT('Ctrl Pts',(2.89180748369484,9.22098281806105,2.29173344131881));
#10277=CARTESIAN_POINT('Ctrl Pts',(3.18016901213384,9.16369115139443,1.8964199105197));
#10278=CARTESIAN_POINT('Ctrl Pts',(3.58482250151549,9.0491078180611,1.02034910224998));
#10279=CARTESIAN_POINT('Ctrl Pts',(3.70091943564033,8.99181615139416,0.539921650446381));
#10280=CARTESIAN_POINT('Ctrl Pts',(3.73951272835577,8.87723281806137,-0.434028630849363));
#10281=CARTESIAN_POINT('Ctrl Pts',(3.66195512441954,8.81994115139465,-0.927168285967855));
#10282=CARTESIAN_POINT('Ctrl Pts',(3.32117934064045,8.70535781806088,-1.85072293885776));
#10283=CARTESIAN_POINT('Ctrl Pts',(3.05805940283662,8.64806615139417,-2.28075974833291));
#10284=CARTESIAN_POINT('Ctrl Pts',(2.38292699958574,8.53348281806136,-3.01047130961474));
#10285=CARTESIAN_POINT('Ctrl Pts',(1.97115272661516,8.47619115139423,-3.30983155424184));
#10286=CARTESIAN_POINT('Ctrl Pts',(1.05919028403238,8.36160781806131,-3.72935184541724));
#10287=CARTESIAN_POINT('Ctrl Pts',(0.559346062977528,8.30431615139426,-3.8493110150021));
#10288=CARTESIAN_POINT('Ctrl Pts',(-0.453453043380547,8.18973281806127,
-3.8879043077944));
#10289=CARTESIAN_POINT('Ctrl Pts',(-0.966009467727636,8.13244115139459,
-3.80648446824784));
#10290=CARTESIAN_POINT('Ctrl Pts',(-1.92545575497591,8.01785781806094,-3.45084188282187));
#10291=CARTESIAN_POINT('Ctrl Pts',(-2.37195330655562,7.96056615139459,-3.17672322869252));
#10292=CARTESIAN_POINT('Ctrl Pts',(-3.12913513552178,7.84598281806096,-2.47412055785955));
#10293=CARTESIAN_POINT('Ctrl Pts',(-3.43949409635991,7.78869115139432,-2.04588554269906));
#10294=CARTESIAN_POINT('Ctrl Pts',(-3.87388118930893,7.67410781806122,-1.09803146582633));
#10295=CARTESIAN_POINT('Ctrl Pts',(-3.9977025943682,7.61681615139413,-0.578770475493801));
#10296=CARTESIAN_POINT('Ctrl Pts',(-4.03629588722871,7.50223281806141,0.472877455896854));
#10297=CARTESIAN_POINT('Ctrl Pts',(-3.95101381207413,7.44494115139464,1.00485064950196));
#10298=CARTESIAN_POINT('Ctrl Pts',(-3.58050442500531,7.33035781806089,2.00018857107951));
#10299=CARTESIAN_POINT('Ctrl Pts',(-3.29538705454006,7.27306615139411,2.46314686479214));
#10300=CARTESIAN_POINT('Ctrl Pts',(-2.56531411614172,7.15848281806142,3.24779896141502));
#10301=CARTESIAN_POINT('Ctrl Pts',(-2.12061835877177,7.10119115139444,3.5691566384858));
#10302=CARTESIAN_POINT('Ctrl Pts',(-1.13687264763148,6.98660781806109,4.01841053319279));
#10303=CARTESIAN_POINT('Ctrl Pts',(-0.598194887996293,6.92931615139405,
4.14609417373796));
#10304=CARTESIAN_POINT('Ctrl Pts',(0.492301868399383,6.81473281806148,4.18468746665935));
#10305=CARTESIAN_POINT('Ctrl Pts',(1.04369183128993,6.75744115139454,4.09554315589853));
#10306=CARTESIAN_POINT('Ctrl Pts',(2.07492138716947,6.64285781806099,3.71016696719063));
#10307=CARTESIAN_POINT('Ctrl Pts',(2.55434042303921,6.585566151395,3.41405088038211));
#10308=CARTESIAN_POINT('Ctrl Pts',(3.36646278729771,6.47098281806054,2.65650767442937));
#10309=CARTESIAN_POINT('Ctrl Pts',(3.69881918061998,6.41369115139488,2.19535117483371));
#10310=CARTESIAN_POINT('Ctrl Pts',(4.16293987706837,6.29910781806065,1.1757138294474));
#10311=CARTESIAN_POINT('Ctrl Pts',(4.29448575311062,6.24181615139464,0.617619300488533));
#10312=CARTESIAN_POINT('Ctrl Pts',(4.3330790460871,6.1272328180609,-0.511726280891663));
#10313=CARTESIAN_POINT('Ctrl Pts',(4.24007249972198,6.06994115139421,-1.0825330130876));
#10314=CARTESIAN_POINT('Ctrl Pts',(3.8398295093769,5.95535781806132,-2.14965420324974));
#10315=CARTESIAN_POINT('Ctrl Pts',(3.53271470621635,5.89806615139432,-2.64553398129709));
#10316=CARTESIAN_POINT('Ctrl Pts',(2.74770123272482,5.78348281806122,-3.48512661316959));
#10317=CARTESIAN_POINT('Ctrl Pts',(2.27008399088731,5.72619115139493,-3.82848172276042));
#10318=CARTESIAN_POINT('Ctrl Pts',(1.21455501127165,5.6116078180606,-4.30746922093769));
#10319=CARTESIAN_POINT('Ctrl Pts',(0.637043712966868,5.55431615139431,-4.44287733248579));
#10320=CARTESIAN_POINT('Ctrl Pts',(-0.531150693370039,5.43973281806122,
-4.48147062551234));
#10321=CARTESIAN_POINT('Ctrl Pts',(-1.12137419490063,5.38244115139481,-4.38460184354212));
#10322=CARTESIAN_POINT('Ctrl Pts',(-2.22438701931463,5.26785781806072,-3.96949205156649));
#10323=CARTESIAN_POINT('Ctrl Pts',(-2.73672753956158,5.21056615139485,-3.651378532048));
#10324=CARTESIAN_POINT('Ctrl Pts',(-3.60379043903486,5.09598281806069,-2.83889479102288));
#10325=CARTESIAN_POINT('Ctrl Pts',(-3.95814426490714,5.03869115139445,-2.34481680693236));
#10326=CARTESIAN_POINT('Ctrl Pts',(-4.45199856480073,4.92410781806109,-1.25339619310446));
#10327=CARTESIAN_POINT('Ctrl Pts',(-4.59126891186371,4.86681615139442,-0.656468125439367));
#10328=CARTESIAN_POINT('Ctrl Pts',(-4.62986220493482,4.75223281806112,0.550575105842595));
#10329=CARTESIAN_POINT('Ctrl Pts',(-4.52913118736181,4.69494115139439,1.1602153767205));
#10330=CARTESIAN_POINT('Ctrl Pts',(-4.09915459375653,4.58035781806114,2.2991198353727));
#10331=CARTESIAN_POINT('Ctrl Pts',(-3.77004235787144,4.52306615139435,2.82792109783747));
#10332=CARTESIAN_POINT('Ctrl Pts',(-2.93008834932913,4.40848281806118,3.72245426488873));
#10333=CARTESIAN_POINT('Ctrl Pts',(-2.41954962296883,4.35119115139434,4.08780680705904));
#10334=CARTESIAN_POINT('Ctrl Pts',(-1.29223737494584,4.2366078180612,4.59652790865858));
#10335=CARTESIAN_POINT('Ctrl Pts',(-0.675892537901207,4.17931615139434,
4.73966049124288));
#10336=CARTESIAN_POINT('Ctrl Pts',(0.569999518304482,4.06473281806119,4.77825378435605));
#10337=CARTESIAN_POINT('Ctrl Pts',(1.19905655854802,4.00744115139456,4.67366053118015));
#10338=CARTESIAN_POINT('Ctrl Pts',(2.37385265142312,3.89285781806098,4.2288171359479));
#10339=CARTESIAN_POINT('Ctrl Pts',(2.91911465611821,3.83556615139452,3.88870618369294));
#10340=CARTESIAN_POINT('Ctrl Pts',(3.84111809073775,3.72098281806102,3.02128190763733));
#10341=CARTESIAN_POINT('Ctrl Pts',(4.21746934921548,3.66369115139447,2.49428243900129));
#10342=CARTESIAN_POINT('Ctrl Pts',(4.74105725251191,3.54910781806106,1.33107855679123));
#10343=CARTESIAN_POINT('Ctrl Pts',(4.88805207062498,3.49181615139418,0.695316950351842));
#10344=CARTESIAN_POINT('Ctrl Pts',(4.92664536377436,3.37723281806136,-0.589423930755165));
#10345=CARTESIAN_POINT('Ctrl Pts',(4.81818987499502,3.31994115139439,-1.23789774038871));
#10346=CARTESIAN_POINT('Ctrl Pts',(4.35847967814275,3.20535781806115,-2.44858546746038));
#10347=CARTESIAN_POINT('Ctrl Pts',(4.00737000950903,3.14806615139448,-3.01030821440669));
#10348=CARTESIAN_POINT('Ctrl Pts',(3.11247546595094,3.03348281806106,-3.95978191657904));
#10349=CARTESIAN_POINT('Ctrl Pts',(2.56901525502413,2.97619115139456,-4.34713189137729));
#10350=CARTESIAN_POINT('Ctrl Pts',(1.36991973864622,2.86160781806097,-4.88558659635986));
#10351=CARTESIAN_POINT('Ctrl Pts',(0.714741362801074,2.80431615139412,-5.0364436500079));
#10352=CARTESIAN_POINT('Ctrl Pts',(-0.608848343204429,2.68973281806141,
-5.07503694319185));
#10353=CARTESIAN_POINT('Ctrl Pts',(-1.27673892223029,2.6324411513943,-4.96271921881158));
#10354=CARTESIAN_POINT('Ctrl Pts',(-2.52331828349673,2.51785781806124,-4.48814222033592));
#10355=CARTESIAN_POINT('Ctrl Pts',(-3.10150177270171,2.46056615139471,-4.12603383532024));
#10356=CARTESIAN_POINT('Ctrl Pts',(-4.0784457424138,2.34598281806081,-3.20366902426941));
#10357=CARTESIAN_POINT('Ctrl Pts',(-4.47679443354355,2.28869115139434,-2.64374807104099));
#10358=CARTESIAN_POINT('Ctrl Pts',(-5.03011594020335,2.1741078180612,-1.40876092050723));
#10359=CARTESIAN_POINT('Ctrl Pts',(-5.18483522939207,2.11681615139406,-0.734165775240769));
#10360=CARTESIAN_POINT('Ctrl Pts',(-5.22342852260808,2.00223281806147,0.628272755644193));
#10361=CARTESIAN_POINT('Ctrl Pts',(-5.10724856262497,1.94494115139452,1.31558010408276));
#10362=CARTESIAN_POINT('Ctrl Pts',(-4.61780476253225,1.83035781806102,2.59805109952221));
#10363=CARTESIAN_POINT('Ctrl Pts',(-4.24469766112837,1.77306615139441,3.1926953310021));
#10364=CARTESIAN_POINT('Ctrl Pts',(-3.29486258259099,1.65848281806113,4.19710956824316));
#10365=CARTESIAN_POINT('Ctrl Pts',(-2.71848088705236,1.60119115139435,4.60645697571289));
#10366=CARTESIAN_POINT('Ctrl Pts',(-1.44760210237368,1.48660781806119,5.17464528404378));
#10367=CARTESIAN_POINT('Ctrl Pts',(-0.753590187674045,1.42931615139403,
5.33322680877775));
#10368=CARTESIAN_POINT('Ctrl Pts',(0.647697168077543,1.3147328180615,5.37182010202281));
#10369=CARTESIAN_POINT('Ctrl Pts',(1.35442128593412,1.25744115139439,5.25177790643984));
#10370=CARTESIAN_POINT('Ctrl Pts',(2.67278391554878,1.14285781806115,4.7474673047271));
#10371=CARTESIAN_POINT('Ctrl Pts',(3.28388888930855,1.08556615139459,4.36336148693201));
#10372=CARTESIAN_POINT('Ctrl Pts',(4.3157733940665,0.970982818060947,3.38605614091702));
#10373=CARTESIAN_POINT('Ctrl Pts',(4.73611951788435,0.913691151394175,2.79321370306255));
#10374=CARTESIAN_POINT('Ctrl Pts',(5.31917462788209,0.79910781806136,1.48644328424131));
#10375=CARTESIAN_POINT('Ctrl Pts',(5.48161838816491,0.741816151394642,0.773014600098004));
#10376=CARTESIAN_POINT('Ctrl Pts',(5.52021168143606,0.627232818060896,-0.667121580501539));
#10377=CARTESIAN_POINT('Ctrl Pts',(5.39630725025002,0.569941151394671,-1.39326246779836));
#10378=CARTESIAN_POINT('Ctrl Pts',(4.87712984692664,0.455357818060863,-2.7475167315625));
#10379=CARTESIAN_POINT('Ctrl Pts',(4.48202531273885,0.398066151394155,-3.37508244761294));
#10380=CARTESIAN_POINT('Ctrl Pts',(3.47724969923989,0.283482818061382,-4.43443721989186));
#10381=CARTESIAN_POINT('Ctrl Pts',(2.8679465190623,0.226191151394174,-4.86578206006134));
#10382=CARTESIAN_POINT('Ctrl Pts',(1.52528446611942,0.111607818061363,-5.46370397171486));
#10383=CARTESIAN_POINT('Ctrl Pts',(0.792439012521748,0.0543161513944402,
-5.63000996755282));
#10384=CARTESIAN_POINT('Ctrl Pts',(-0.686545992925361,-0.0602671819389035,
-5.66860326084855));
#10385=CARTESIAN_POINT('Ctrl Pts',(-1.43210364967231,-0.117558848605399,
-5.54083659405887));
#10386=CARTESIAN_POINT('Ctrl Pts',(-2.82224954756648,-0.232142181939065,
-5.00679238912752));
#10387=CARTESIAN_POINT('Ctrl Pts',(-3.46627599744854,-0.28943384860568,
-4.6006891460729));
#10388=CARTESIAN_POINT('Ctrl Pts',(-4.0096885258173,-0.346725515272232,
-4.08456619805421));
#10389=CARTESIAN_POINT('Ctrl Pts',(-2.36559314293001,11.,-2.37295192838617));
#10390=CARTESIAN_POINT('Ctrl Pts',(-2.68495589138643,10.9427083333325,-2.0720405595763));
#10391=CARTESIAN_POINT('Ctrl Pts',(-2.94612920879841,10.8854166666664,-1.70595228936294));
#10392=CARTESIAN_POINT('Ctrl Pts',(-3.30964371429254,10.7708333333336,-0.896538039613314));
#10393=CARTESIAN_POINT('Ctrl Pts',(-3.41180604852602,10.7135416666669,-0.453515668913589));
#10394=CARTESIAN_POINT('Ctrl Pts',(-3.4379002366457,10.5989583333331,0.443108774718904));
#10395=CARTESIAN_POINT('Ctrl Pts',(-3.36178304590245,10.5416666666666,0.896358100460257));
#10396=CARTESIAN_POINT('Ctrl Pts',(-3.03905091217473,10.4270833333334,1.74368979436799));
#10397=CARTESIAN_POINT('Ctrl Pts',(-2.79252711081109,10.3697916666664,2.13742396723561));
#10398=CARTESIAN_POINT('Ctrl Pts',(-2.16323413009096,10.2552083333337,2.80361970275416));
#10399=CARTESIAN_POINT('Ctrl Pts',(-1.78068510549046,10.1979166666664,3.07579175088966));
#10400=CARTESIAN_POINT('Ctrl Pts',(-0.935379221363662,10.0833333333336,
3.45417305821104));
#10401=CARTESIAN_POINT('Ctrl Pts',(-0.472940081479242,10.0260416666666,
3.56019762788479));
#10402=CARTESIAN_POINT('Ctrl Pts',(0.462533187284589,9.91145833333345,3.58629181608734));
#10403=CARTESIAN_POINT('Ctrl Pts',(0.935199282188079,9.85416666666669,3.50631238974053));
#10404=CARTESIAN_POINT('Ctrl Pts',(1.81842261051809,9.73958333333332,3.16871345434639));
#10405=CARTESIAN_POINT('Ctrl Pts',(2.22861752543397,9.68229166666673,2.91119093668731));
#10406=CARTESIAN_POINT('Ctrl Pts',(2.92228352868554,9.56770833333328,2.25442768834444));
#10407=CARTESIAN_POINT('Ctrl Pts',(3.20545429299277,9.51041666666666,1.85541792160244));
#10408=CARTESIAN_POINT('Ctrl Pts',(3.59870240211769,9.39583333333334,0.974220403129539));
#10409=CARTESIAN_POINT('Ctrl Pts',(3.70858920724845,9.3385416666664,0.492364494026195));
#10410=CARTESIAN_POINT('Ctrl Pts',(3.73468339552408,9.22395833333361,-0.481957599831572));
#10411=CARTESIAN_POINT('Ctrl Pts',(3.65084173357628,9.16666666666689,-0.974040463933888));
#10412=CARTESIAN_POINT('Ctrl Pts',(3.29837599652037,9.05208333333312,-1.8931554266502));
#10413=CARTESIAN_POINT('Ctrl Pts',(3.02985476255422,8.99479166666641,-2.31981108364774));
#10414=CARTESIAN_POINT('Ctrl Pts',(2.34562124660724,8.8802083333336,-3.04094735460153));
#10415=CARTESIAN_POINT('Ctrl Pts',(1.93015073770027,8.82291666666647,-3.33511683510577));
#10416=CARTESIAN_POINT('Ctrl Pts',(1.01306158490958,8.70833333333354,-3.74323174601444));
#10417=CARTESIAN_POINT('Ctrl Pts',(0.511788906557484,8.6510416666665,-3.85698078661577));
#10418=CARTESIAN_POINT('Ctrl Pts',(-0.501382012362897,8.53645833333351,
-3.88307497495716));
#10419=CARTESIAN_POINT('Ctrl Pts',(-1.01288164569554,8.47916666666683,-3.79537107740945));
#10420=CARTESIAN_POINT('Ctrl Pts',(-1.96788824276646,8.36458333333318,-3.42803853869692));
#10421=CARTESIAN_POINT('Ctrl Pts',(-2.41100464187403,8.30729166666683,-3.14851858841386));
#10422=CARTESIAN_POINT('Ctrl Pts',(-3.159611180505,8.1927083333332,-2.43681480487731));
#10423=CARTESIAN_POINT('Ctrl Pts',(-3.46477937722837,8.13541666666656,-2.00488355378617));
#10424=CARTESIAN_POINT('Ctrl Pts',(-3.8877610899016,8.02083333333345,-1.05190276670153));
#10425=CARTESIAN_POINT('Ctrl Pts',(-4.00537236598643,7.96354166666637,-0.531213319073915));
#10426=CARTESIAN_POINT('Ctrl Pts',(-4.03146655438691,7.84895833333365,0.520806424879362));
#10427=CARTESIAN_POINT('Ctrl Pts',(-3.93990042124014,7.79166666666665,1.05172282747159));
#10428=CARTESIAN_POINT('Ctrl Pts',(-3.55770108087595,7.67708333333337,2.04262105886835));
#10429=CARTESIAN_POINT('Ctrl Pts',(-3.26718241426475,7.61979166666659,2.50219820011361));
#10430=CARTESIAN_POINT('Ctrl Pts',(-2.52800836315612,7.50520833333343,3.27827500639517));
#10431=CARTESIAN_POINT('Ctrl Pts',(-2.07961636986072,7.44791666666668,3.59444191935829));
#10432=CARTESIAN_POINT('Ctrl Pts',(-1.09074394850484,7.33333333333333,4.03229043378143));
#10433=CARTESIAN_POINT('Ctrl Pts',(-0.550637731576509,7.27604166666629,
4.15376394536062));
#10434=CARTESIAN_POINT('Ctrl Pts',(0.540230837381994,7.16145833333372,4.17985813381312));
#10435=CARTESIAN_POINT('Ctrl Pts',(1.09056400926098,7.10416666666678,4.08442976506864));
#10436=CARTESIAN_POINT('Ctrl Pts',(2.11735387495688,6.98958333333323,3.68736362305719));
#10437=CARTESIAN_POINT('Ctrl Pts',(2.59339175836345,6.93229166666724,3.38584624010982));
#10438=CARTESIAN_POINT('Ctrl Pts',(3.3969388322751,6.81770833333277,2.61920192144075));
#10439=CARTESIAN_POINT('Ctrl Pts',(3.72410446149635,6.76041666666712,2.15434918592434));
#10440=CARTESIAN_POINT('Ctrl Pts',(4.17681977765313,6.64583333333289,1.12958513031907));
#10441=CARTESIAN_POINT('Ctrl Pts',(4.30215552473732,6.58854166666688,0.570062144068889));
#10442=CARTESIAN_POINT('Ctrl Pts',(4.32824971323683,6.47395833333313,-0.559655249874413));
#10443=CARTESIAN_POINT('Ctrl Pts',(4.22895910889563,6.41666666666645,-1.12940519106012));
#10444=CARTESIAN_POINT('Ctrl Pts',(3.81702616523991,6.30208333333356,-2.19208669103568));
#10445=CARTESIAN_POINT('Ctrl Pts',(3.50451006594675,6.24479166666656,-2.68458531662391));
#10446=CARTESIAN_POINT('Ctrl Pts',(2.71039547973352,6.13020833333345,-3.51560265814439));
#10447=CARTESIAN_POINT('Ctrl Pts',(2.22908200197935,6.07291666666717,-3.85376700363998));
#10448=CARTESIAN_POINT('Ctrl Pts',(1.16842631214193,5.95833333333284,-4.32134912151925));
#10449=CARTESIAN_POINT('Ctrl Pts',(0.589486556547344,5.90104166666655,-4.45054710411593));
#10450=CARTESIAN_POINT('Ctrl Pts',(-0.579079662352908,5.78645833333346,
-4.47664129265863));
#10451=CARTESIAN_POINT('Ctrl Pts',(-1.16824637287424,5.72916666666705,-4.37348845271886));
#10452=CARTESIAN_POINT('Ctrl Pts',(-2.26681950709949,5.61458333333296,-3.94668870742641));
#10453=CARTESIAN_POINT('Ctrl Pts',(-2.77577887489086,5.55729166666709,-3.62317389178086));
#10454=CARTESIAN_POINT('Ctrl Pts',(-3.6342664840072,5.44270833333292,-2.80158903802911));
#10455=CARTESIAN_POINT('Ctrl Pts',(-3.98342954578962,5.38541666666669,-2.30381481802579));
#10456=CARTESIAN_POINT('Ctrl Pts',(-4.46587846537937,5.27083333333332,-1.20726749397333));
#10457=CARTESIAN_POINT('Ctrl Pts',(-4.59893868349712,5.21354166666665,-0.608910969019916));
#10458=CARTESIAN_POINT('Ctrl Pts',(-4.62503287207784,5.09895833333335,0.598504074825539));
#10459=CARTESIAN_POINT('Ctrl Pts',(-4.51801779654147,5.04166666666663,1.20708755469526));
#10460=CARTESIAN_POINT('Ctrl Pts',(-4.07635124961353,4.92708333333338,2.34155232315641));
#10461=CARTESIAN_POINT('Ctrl Pts',(-3.74183771760646,4.86979166666659,2.86697243316876));
#10462=CARTESIAN_POINT('Ctrl Pts',(-2.89278259633321,4.75520833333342,3.75293030985906));
#10463=CARTESIAN_POINT('Ctrl Pts',(-2.37854763406351,4.69791666666658,4.1130920879442));
#10464=CARTESIAN_POINT('Ctrl Pts',(-1.24610867581347,4.58333333333343,4.61040780923455));
#10465=CARTESIAN_POINT('Ctrl Pts',(-0.628335381481812,4.52604166666658,
4.74733026287932));
#10466=CARTESIAN_POINT('Ctrl Pts',(0.617928487287482,4.41145833333343,4.77342445149605));
#10467=CARTESIAN_POINT('Ctrl Pts',(1.24592873652376,4.35416666666679,4.66254714036264));
#10468=CARTESIAN_POINT('Ctrl Pts',(2.41628513920584,4.23958333333322,4.20601379180208));
#10469=CARTESIAN_POINT('Ctrl Pts',(2.95816599145146,4.18229166666676,3.86050154342994));
#10470=CARTESIAN_POINT('Ctrl Pts',(3.87159413570613,4.06770833333325,2.98397615463943));
#10471=CARTESIAN_POINT('Ctrl Pts',(4.24275463010319,4.01041666666671,2.45328045009706));
#10472=CARTESIAN_POINT('Ctrl Pts',(4.75493715308532,3.8958333333333,1.28494985765777));
#10473=CARTESIAN_POINT('Ctrl Pts',(4.89572184226387,3.83854166666642,0.647759793932574));
#10474=CARTESIAN_POINT('Ctrl Pts',(4.9218160309119,3.72395833333359,-0.637352899738291));
#10475=CARTESIAN_POINT('Ctrl Pts',(4.80707648417982,3.66666666666662,-1.28476991836542));
#10476=CARTESIAN_POINT('Ctrl Pts',(4.33567633399462,3.55208333333339,-2.49101795524214));
#10477=CARTESIAN_POINT('Ctrl Pts',(3.97916536924807,3.49479166666671,-3.04935954974168));
#10478=CARTESIAN_POINT('Ctrl Pts',(3.075169712951,3.38020833333329,-3.99025796154567));
#10479=CARTESIAN_POINT('Ctrl Pts',(2.52801326612096,3.3229166666668,-4.37241717226731));
#10480=CARTESIAN_POINT('Ctrl Pts',(1.3237910395117,3.20833333333321,-4.89946649693097));
#10481=CARTESIAN_POINT('Ctrl Pts',(0.667184206381905,3.15104166666636,-5.04411342164931));
#10482=CARTESIAN_POINT('Ctrl Pts',(-0.656777312187654,3.03645833333365,
-5.07020761032686));
#10483=CARTESIAN_POINT('Ctrl Pts',(-1.32361110020785,2.97916666666654,-4.95160582799841));
#10484=CARTESIAN_POINT('Ctrl Pts',(-2.56575077127763,2.86458333333347,-4.46533887618575));
#10485=CARTESIAN_POINT('Ctrl Pts',(-3.1405531080382,2.80729166666695,-4.09782919506089));
#10486=CARTESIAN_POINT('Ctrl Pts',(-4.10892178737893,2.69270833333305,-3.16636327126786));
#10487=CARTESIAN_POINT('Ctrl Pts',(-4.50207971443576,2.63541666666658,-2.60274608213879));
#10488=CARTESIAN_POINT('Ctrl Pts',(-5.04399584077227,2.52083333333343,-1.36263222137173));
#10489=CARTESIAN_POINT('Ctrl Pts',(-5.1925050010359,2.4635416666663,-0.686608618821642));
#10490=CARTESIAN_POINT('Ctrl Pts',(-5.21859918974068,2.34895833333371,0.67620172462746));
#10491=CARTESIAN_POINT('Ctrl Pts',(-5.09613517181383,2.29166666666676,1.36245228206106));
#10492=CARTESIAN_POINT('Ctrl Pts',(-4.59500141838005,2.17708333333325,2.64048358730238));
#10493=CARTESIAN_POINT('Ctrl Pts',(-4.21649302087059,2.11979166666664,3.23174666634004));
#10494=CARTESIAN_POINT('Ctrl Pts',(-3.25755682958786,2.00520833333337,4.22758561320685));
#10495=CARTESIAN_POINT('Ctrl Pts',(-2.67747889815098,1.94791666666658,4.63174225660692));
#10496=CARTESIAN_POINT('Ctrl Pts',(-1.40147340323737,1.83333333333343,5.18852518461089));
#10497=CARTESIAN_POINT('Ctrl Pts',(-0.706033031254986,1.77604166666627,
5.34089658042353));
#10498=CARTESIAN_POINT('Ctrl Pts',(0.695626137060878,1.66145833333374,5.36699076915345));
#10499=CARTESIAN_POINT('Ctrl Pts',(1.40129346391331,1.60416666666663,5.24066451563091));
#10500=CARTESIAN_POINT('Ctrl Pts',(2.71521640332806,1.48958333333338,4.7246639605727));
#10501=CARTESIAN_POINT('Ctrl Pts',(3.32294022464786,1.43229166666683,4.33515684667557));
#10502=CARTESIAN_POINT('Ctrl Pts',(4.34624943902881,1.31770833333318,3.34875038791256));
#10503=CARTESIAN_POINT('Ctrl Pts',(4.76140479878007,1.26041666666641,2.75221171416214));
#10504=CARTESIAN_POINT('Ctrl Pts',(5.3330545284475,1.1458333333336,1.44031458510402));
#10505=CARTESIAN_POINT('Ctrl Pts',(5.48928815981245,1.08854166666688,0.72545744367903));
#10506=CARTESIAN_POINT('Ctrl Pts',(5.51538234856494,0.973958333333134,-0.715050549484959));
#10507=CARTESIAN_POINT('Ctrl Pts',(5.38519385944284,0.916666666666909,-1.44013464577813));
#10508=CARTESIAN_POINT('Ctrl Pts',(4.85432650277048,0.8020833333331,-2.7899492193412));
#10509=CARTESIAN_POINT('Ctrl Pts',(4.4538206724838,0.744791666666392,-3.4141337829535));
#10510=CARTESIAN_POINT('Ctrl Pts',(3.43994394623404,0.630208333333619,-4.46491326485293));
#10511=CARTESIAN_POINT('Ctrl Pts',(2.82694453016243,0.572916666666411,-4.89106734095877));
#10512=CARTESIAN_POINT('Ctrl Pts',(1.47915576698159,0.4583333333336,-5.47758387227856));
#10513=CARTESIAN_POINT('Ctrl Pts',(0.744881856102772,0.401041666666677,
-5.63767973920226));
#10514=CARTESIAN_POINT('Ctrl Pts',(-0.73447496190878,0.286458333333334,
-5.66377392797554));
#10515=CARTESIAN_POINT('Ctrl Pts',(-1.4789758276525,0.229166666666838,-5.52972320325324));
#10516=CARTESIAN_POINT('Ctrl Pts',(-2.86468203534475,0.114583333333173,
-4.9839890449698));
#10517=CARTESIAN_POINT('Ctrl Pts',(-3.50532733285514,0.0572916666665569,
-4.5724845058884));
#10518=CARTESIAN_POINT('Ctrl Pts',(-4.04445221596811,5.20417042793042E-15,
-4.05181100142375));
#10519=CARTESIAN_POINT('Origin',(-3.92444263558561,5.20417042793042E-15,
-3.92444263558507));
#10520=CARTESIAN_POINT('Origin',(-3.92444263558561,5.20417042793042E-15,
-3.92444263558507));
#10521=CARTESIAN_POINT('',(0.341364976304836,0.056894162717681,30.));
#10522=CARTESIAN_POINT('',(0.141364976304842,0.0568941627176771,30.));
#10523=CARTESIAN_POINT('',(0.741364976304842,0.0568941627176797,30.));
#10524=CARTESIAN_POINT('',(-12.6586350236952,0.0568941627176801,30.));
#10525=CARTESIAN_POINT('',(-5.58363502369516,0.056894162717681,30.));
#10526=CARTESIAN_POINT('',(-25.2086350236952,0.0568941627176813,30.));
#10527=CARTESIAN_POINT('',(17.9913649763048,0.0568941627176905,30.));
#10528=CARTESIAN_POINT('',(16.3413649763048,0.0568941627176911,30.));
#10529=CARTESIAN_POINT('',(-14.0336350236952,0.0568941627176831,30.));
#10530=UNCERTAINTY_MEASURE_WITH_UNIT(LENGTH_MEASURE(0.01),#10552,
'DISTANCE_ACCURACY_VALUE',
'Maximum model space distance between geometric entities at asserted c
onnectivities');
#10531=UNCERTAINTY_MEASURE_WITH_UNIT(LENGTH_MEASURE(0.01),#10552,
'DISTANCE_ACCURACY_VALUE',
'Maximum model space distance between geometric entities at asserted c
onnectivities');
#10532=UNCERTAINTY_MEASURE_WITH_UNIT(LENGTH_MEASURE(0.01),#10552,
'DISTANCE_ACCURACY_VALUE',
'Maximum model space distance between geometric entities at asserted c
onnectivities');
#10533=UNCERTAINTY_MEASURE_WITH_UNIT(LENGTH_MEASURE(0.01),#10552,
'DISTANCE_ACCURACY_VALUE',
'Maximum model space distance between geometric entities at asserted c
onnectivities');
#10534=UNCERTAINTY_MEASURE_WITH_UNIT(LENGTH_MEASURE(0.01),#10552,
'DISTANCE_ACCURACY_VALUE',
'Maximum model space distance between geometric entities at asserted c
onnectivities');
#10535=UNCERTAINTY_MEASURE_WITH_UNIT(LENGTH_MEASURE(0.01),#10552,
'DISTANCE_ACCURACY_VALUE',
'Maximum model space distance between geometric entities at asserted c
onnectivities');
#10536=UNCERTAINTY_MEASURE_WITH_UNIT(LENGTH_MEASURE(0.01),#10552,
'DISTANCE_ACCURACY_VALUE',
'Maximum model space distance between geometric entities at asserted c
onnectivities');
#10537=UNCERTAINTY_MEASURE_WITH_UNIT(LENGTH_MEASURE(0.01),#10552,
'DISTANCE_ACCURACY_VALUE',
'Maximum model space distance between geometric entities at asserted c
onnectivities');
#10538=UNCERTAINTY_MEASURE_WITH_UNIT(LENGTH_MEASURE(0.01),#10552,
'DISTANCE_ACCURACY_VALUE',
'Maximum model space distance between geometric entities at asserted c
onnectivities');
#10539=UNCERTAINTY_MEASURE_WITH_UNIT(LENGTH_MEASURE(0.01),#10552,
'DISTANCE_ACCURACY_VALUE',
'Maximum model space distance between geometric entities at asserted c
onnectivities');
#10540=UNCERTAINTY_MEASURE_WITH_UNIT(LENGTH_MEASURE(0.01),#10552,
'DISTANCE_ACCURACY_VALUE',
'Maximum model space distance between geometric entities at asserted c
onnectivities');
#10541=(
GEOMETRIC_REPRESENTATION_CONTEXT(3)
GLOBAL_UNCERTAINTY_ASSIGNED_CONTEXT((#10530))
GLOBAL_UNIT_ASSIGNED_CONTEXT((#10552,#10554,#10555))
REPRESENTATION_CONTEXT('','3D')
);
#10542=(
GEOMETRIC_REPRESENTATION_CONTEXT(3)
GLOBAL_UNCERTAINTY_ASSIGNED_CONTEXT((#10531))
GLOBAL_UNIT_ASSIGNED_CONTEXT((#10552,#10554,#10555))
REPRESENTATION_CONTEXT('','3D')
);
#10543=(
GEOMETRIC_REPRESENTATION_CONTEXT(3)
GLOBAL_UNCERTAINTY_ASSIGNED_CONTEXT((#10532))
GLOBAL_UNIT_ASSIGNED_CONTEXT((#10552,#10554,#10555))
REPRESENTATION_CONTEXT('','3D')
);
#10544=(
GEOMETRIC_REPRESENTATION_CONTEXT(3)
GLOBAL_UNCERTAINTY_ASSIGNED_CONTEXT((#10533))
GLOBAL_UNIT_ASSIGNED_CONTEXT((#10552,#10554,#10555))
REPRESENTATION_CONTEXT('','3D')
);
#10545=(
GEOMETRIC_REPRESENTATION_CONTEXT(3)
GLOBAL_UNCERTAINTY_ASSIGNED_CONTEXT((#10534))
GLOBAL_UNIT_ASSIGNED_CONTEXT((#10552,#10554,#10555))
REPRESENTATION_CONTEXT('','3D')
);
#10546=(
GEOMETRIC_REPRESENTATION_CONTEXT(3)
GLOBAL_UNCERTAINTY_ASSIGNED_CONTEXT((#10535))
GLOBAL_UNIT_ASSIGNED_CONTEXT((#10552,#10554,#10555))
REPRESENTATION_CONTEXT('','3D')
);
#10547=(
GEOMETRIC_REPRESENTATION_CONTEXT(3)
GLOBAL_UNCERTAINTY_ASSIGNED_CONTEXT((#10536))
GLOBAL_UNIT_ASSIGNED_CONTEXT((#10552,#10554,#10555))
REPRESENTATION_CONTEXT('','3D')
);
#10548=(
GEOMETRIC_REPRESENTATION_CONTEXT(3)
GLOBAL_UNCERTAINTY_ASSIGNED_CONTEXT((#10537))
GLOBAL_UNIT_ASSIGNED_CONTEXT((#10552,#10554,#10555))
REPRESENTATION_CONTEXT('','3D')
);
#10549=(
GEOMETRIC_REPRESENTATION_CONTEXT(3)
GLOBAL_UNCERTAINTY_ASSIGNED_CONTEXT((#10538))
GLOBAL_UNIT_ASSIGNED_CONTEXT((#10552,#10554,#10555))
REPRESENTATION_CONTEXT('','3D')
);
#10550=(
GEOMETRIC_REPRESENTATION_CONTEXT(3)
GLOBAL_UNCERTAINTY_ASSIGNED_CONTEXT((#10539))
GLOBAL_UNIT_ASSIGNED_CONTEXT((#10552,#10554,#10555))
REPRESENTATION_CONTEXT('','3D')
);
#10551=(
GEOMETRIC_REPRESENTATION_CONTEXT(3)
GLOBAL_UNCERTAINTY_ASSIGNED_CONTEXT((#10540))
GLOBAL_UNIT_ASSIGNED_CONTEXT((#10552,#10554,#10555))
REPRESENTATION_CONTEXT('','3D')
);
#10552=(
LENGTH_UNIT()
NAMED_UNIT(*)
SI_UNIT(.MILLI.,.METRE.)
);
#10553=(
LENGTH_UNIT()
NAMED_UNIT(*)
SI_UNIT($,.METRE.)
);
#10554=(
NAMED_UNIT(*)
PLANE_ANGLE_UNIT()
SI_UNIT($,.RADIAN.)
);
#10555=(
NAMED_UNIT(*)
SI_UNIT($,.STERADIAN.)
SOLID_ANGLE_UNIT()
);
#10556=SHAPE_DEFINITION_REPRESENTATION(#10566,#10585);
#10557=SHAPE_DEFINITION_REPRESENTATION(#10567,#10586);
#10558=SHAPE_DEFINITION_REPRESENTATION(#10568,#10587);
#10559=SHAPE_DEFINITION_REPRESENTATION(#10569,#10588);
#10560=SHAPE_DEFINITION_REPRESENTATION(#10570,#10589);
#10561=SHAPE_DEFINITION_REPRESENTATION(#10571,#10590);
#10562=SHAPE_DEFINITION_REPRESENTATION(#10572,#10591);
#10563=SHAPE_DEFINITION_REPRESENTATION(#10573,#10592);
#10564=SHAPE_DEFINITION_REPRESENTATION(#10574,#10593);
#10565=SHAPE_DEFINITION_REPRESENTATION(#10575,#10594);
#10566=PRODUCT_DEFINITION_SHAPE('',$,#10596);
#10567=PRODUCT_DEFINITION_SHAPE('',$,#10597);
#10568=PRODUCT_DEFINITION_SHAPE('',$,#10598);
#10569=PRODUCT_DEFINITION_SHAPE('',$,#10599);
#10570=PRODUCT_DEFINITION_SHAPE('',$,#10600);
#10571=PRODUCT_DEFINITION_SHAPE('',$,#10601);
#10572=PRODUCT_DEFINITION_SHAPE('',$,#10602);
#10573=PRODUCT_DEFINITION_SHAPE('',$,#10603);
#10574=PRODUCT_DEFINITION_SHAPE('',$,#10604);
#10575=PRODUCT_DEFINITION_SHAPE('',$,#10605);
#10576=PRODUCT_DEFINITION_SHAPE($,$,#38);
#10577=PRODUCT_DEFINITION_SHAPE($,$,#39);
#10578=PRODUCT_DEFINITION_SHAPE($,$,#40);
#10579=PRODUCT_DEFINITION_SHAPE($,$,#41);
#10580=PRODUCT_DEFINITION_SHAPE($,$,#42);
#10581=PRODUCT_DEFINITION_SHAPE($,$,#43);
#10582=PRODUCT_DEFINITION_SHAPE($,$,#44);
#10583=PRODUCT_DEFINITION_SHAPE($,$,#45);
#10584=PRODUCT_DEFINITION_SHAPE($,$,#46);
#10585=SHAPE_REPRESENTATION('',(#3536,#4027,#4028,#4029,#4030,#4031,#4032,
#4033,#4034,#4035),#10541);
#10586=SHAPE_REPRESENTATION('',(#3537),#10542);
#10587=SHAPE_REPRESENTATION('',(#3577),#10543);
#10588=SHAPE_REPRESENTATION('',(#3624),#10544);
#10589=SHAPE_REPRESENTATION('',(#3633),#10545);
#10590=SHAPE_REPRESENTATION('',(#3651),#10546);
#10591=SHAPE_REPRESENTATION('',(#3691),#10547);
#10592=SHAPE_REPRESENTATION('',(#3718),#10548);
#10593=SHAPE_REPRESENTATION('',(#4012),#10549);
#10594=SHAPE_REPRESENTATION('',(#4016),#10550);
#10595=PRODUCT_DEFINITION_CONTEXT('part definition',#10627,'design');
#10596=PRODUCT_DEFINITION('MAT-038','MAT-038',#10606,#10595);
#10597=PRODUCT_DEFINITION('Housing','Housing',#10607,#10595);
#10598=PRODUCT_DEFINITION('Core','Core',#10608,#10595);
#10599=PRODUCT_DEFINITION('Coil','Coil',#10609,#10595);
#10600=PRODUCT_DEFINITION('Housing cover','Housing Cover',#10610,#10595);
#10601=PRODUCT_DEFINITION('Plunger','Plunger',#10611,#10595);
#10602=PRODUCT_DEFINITION('Washer','Washer',#10612,#10595);
#10603=PRODUCT_DEFINITION('Nut','Nut',#10613,#10595);
#10604=PRODUCT_DEFINITION('Rubber Seal','Rubber Seal',#10614,#10595);
#10605=PRODUCT_DEFINITION('spring','Spring',#10615,#10595);
#10606=PRODUCT_DEFINITION_FORMATION('',$,#10629);
#10607=PRODUCT_DEFINITION_FORMATION('',$,#10630);
#10608=PRODUCT_DEFINITION_FORMATION('',$,#10631);
#10609=PRODUCT_DEFINITION_FORMATION('',$,#10632);
#10610=PRODUCT_DEFINITION_FORMATION('',$,#10633);
#10611=PRODUCT_DEFINITION_FORMATION('',$,#10634);
#10612=PRODUCT_DEFINITION_FORMATION('',$,#10635);
#10613=PRODUCT_DEFINITION_FORMATION('',$,#10636);
#10614=PRODUCT_DEFINITION_FORMATION('',$,#10637);
#10615=PRODUCT_DEFINITION_FORMATION('',$,#10638);
#10616=PRODUCT_RELATED_PRODUCT_CATEGORY('MAT-038','MAT-038',(#10629));
#10617=PRODUCT_RELATED_PRODUCT_CATEGORY('Housing','Housing',(#10630));
#10618=PRODUCT_RELATED_PRODUCT_CATEGORY('Core','Core',(#10631));
#10619=PRODUCT_RELATED_PRODUCT_CATEGORY('Coil','Coil',(#10632));
#10620=PRODUCT_RELATED_PRODUCT_CATEGORY('Housing Cover','Housing Cover',
(#10633));
#10621=PRODUCT_RELATED_PRODUCT_CATEGORY('Plunger','Plunger',(#10634));
#10622=PRODUCT_RELATED_PRODUCT_CATEGORY('Washer','Washer',(#10635));
#10623=PRODUCT_RELATED_PRODUCT_CATEGORY('Nut','Nut',(#10636));
#10624=PRODUCT_RELATED_PRODUCT_CATEGORY('Rubber Seal','Rubber Seal',(#10637));
#10625=PRODUCT_RELATED_PRODUCT_CATEGORY('Spring','Spring',(#10638));
#10626=APPLICATION_PROTOCOL_DEFINITION('international standard',
'automotive_design',2009,#10627);
#10627=APPLICATION_CONTEXT(
'Core Data for Automotive Mechanical Design Process');
#10628=PRODUCT_CONTEXT('part definition',#10627,'mechanical');
#10629=PRODUCT('MAT-038','MAT-038','STEP AP214',(#10628));
#10630=PRODUCT('Housing','Housing','Housing',(#10628));
#10631=PRODUCT('Core','Core',$,(#10628));
#10632=PRODUCT('Coil','Coil',$,(#10628));
#10633=PRODUCT('Housing cover','Housing Cover',$,(#10628));
#10634=PRODUCT('Plunger','Plunger',$,(#10628));
#10635=PRODUCT('Washer','Washer',$,(#10628));
#10636=PRODUCT('Nut','Nut',$,(#10628));
#10637=PRODUCT('Rubber Seal','Rubber Seal',$,(#10628));
#10638=PRODUCT('spring','Spring',$,(#10628));
#10639=PRESENTATION_STYLE_ASSIGNMENT((#10646));
#10640=PRESENTATION_STYLE_ASSIGNMENT((#10647));
#10641=PRESENTATION_STYLE_ASSIGNMENT((#10648));
#10642=PRESENTATION_STYLE_ASSIGNMENT((#10649));
#10643=PRESENTATION_STYLE_ASSIGNMENT((#10650));
#10644=PRESENTATION_STYLE_ASSIGNMENT((#10651));
#10645=PRESENTATION_STYLE_ASSIGNMENT((#10652));
#10646=SURFACE_STYLE_USAGE(.BOTH.,#10653);
#10647=SURFACE_STYLE_USAGE(.BOTH.,#10654);
#10648=SURFACE_STYLE_USAGE(.BOTH.,#10655);
#10649=SURFACE_STYLE_USAGE(.BOTH.,#10656);
#10650=SURFACE_STYLE_USAGE(.BOTH.,#10657);
#10651=SURFACE_STYLE_USAGE(.BOTH.,#10658);
#10652=SURFACE_STYLE_USAGE(.BOTH.,#10659);
#10653=SURFACE_SIDE_STYLE('',(#10660));
#10654=SURFACE_SIDE_STYLE('',(#10661));
#10655=SURFACE_SIDE_STYLE('',(#10662));
#10656=SURFACE_SIDE_STYLE('',(#10663));
#10657=SURFACE_SIDE_STYLE('',(#10664));
#10658=SURFACE_SIDE_STYLE('',(#10665));
#10659=SURFACE_SIDE_STYLE('',(#10666));
#10660=SURFACE_STYLE_FILL_AREA(#10667);
#10661=SURFACE_STYLE_FILL_AREA(#10668);
#10662=SURFACE_STYLE_FILL_AREA(#10669);
#10663=SURFACE_STYLE_FILL_AREA(#10670);
#10664=SURFACE_STYLE_FILL_AREA(#10671);
#10665=SURFACE_STYLE_FILL_AREA(#10672);
#10666=SURFACE_STYLE_FILL_AREA(#10673);
#10667=FILL_AREA_STYLE('Steel - Satin',(#10674));
#10668=FILL_AREA_STYLE('Opaque(20,51,87)',(#10675));
#10669=FILL_AREA_STYLE('Opaque(97,158,199)',(#10676));
#10670=FILL_AREA_STYLE('Opaque(227,224,212)',(#10677));
#10671=FILL_AREA_STYLE('Opaque(61,176,222)',(#10678));
#10672=FILL_AREA_STYLE('Opaque(31,36,43)',(#10679));
#10673=FILL_AREA_STYLE('Opaque(122,133,145)',(#10680));
#10674=FILL_AREA_STYLE_COLOUR('Steel - Satin',#10681);
#10675=FILL_AREA_STYLE_COLOUR('Opaque(20,51,87)',#10682);
#10676=FILL_AREA_STYLE_COLOUR('Opaque(97,158,199)',#10683);
#10677=FILL_AREA_STYLE_COLOUR('Opaque(227,224,212)',#10684);
#10678=FILL_AREA_STYLE_COLOUR('Opaque(61,176,222)',#10685);
#10679=FILL_AREA_STYLE_COLOUR('Opaque(31,36,43)',#10686);
#10680=FILL_AREA_STYLE_COLOUR('Opaque(122,133,145)',#10687);
#10681=COLOUR_RGB('Steel - Satin',0.627450980392157,0.627450980392157,0.627450980392157);
#10682=COLOUR_RGB('Opaque(20,51,87)',0.0784313725490196,0.2,0.341176470588235);
#10683=COLOUR_RGB('Opaque(97,158,199)',0.380392156862745,0.619607843137255,
0.780392156862745);
#10684=COLOUR_RGB('Opaque(227,224,212)',0.890196078431372,0.87843137254902,
0.831372549019608);
#10685=COLOUR_RGB('Opaque(61,176,222)',0.23921568627451,0.690196078431373,
0.870588235294118);
#10686=COLOUR_RGB('Opaque(31,36,43)',0.12156862745098,0.141176470588235,
0.168627450980392);
#10687=COLOUR_RGB('Opaque(122,133,145)',0.47843137254902,0.52156862745098,
0.568627450980392);
ENDSEC;
END-ISO-10303-21;
